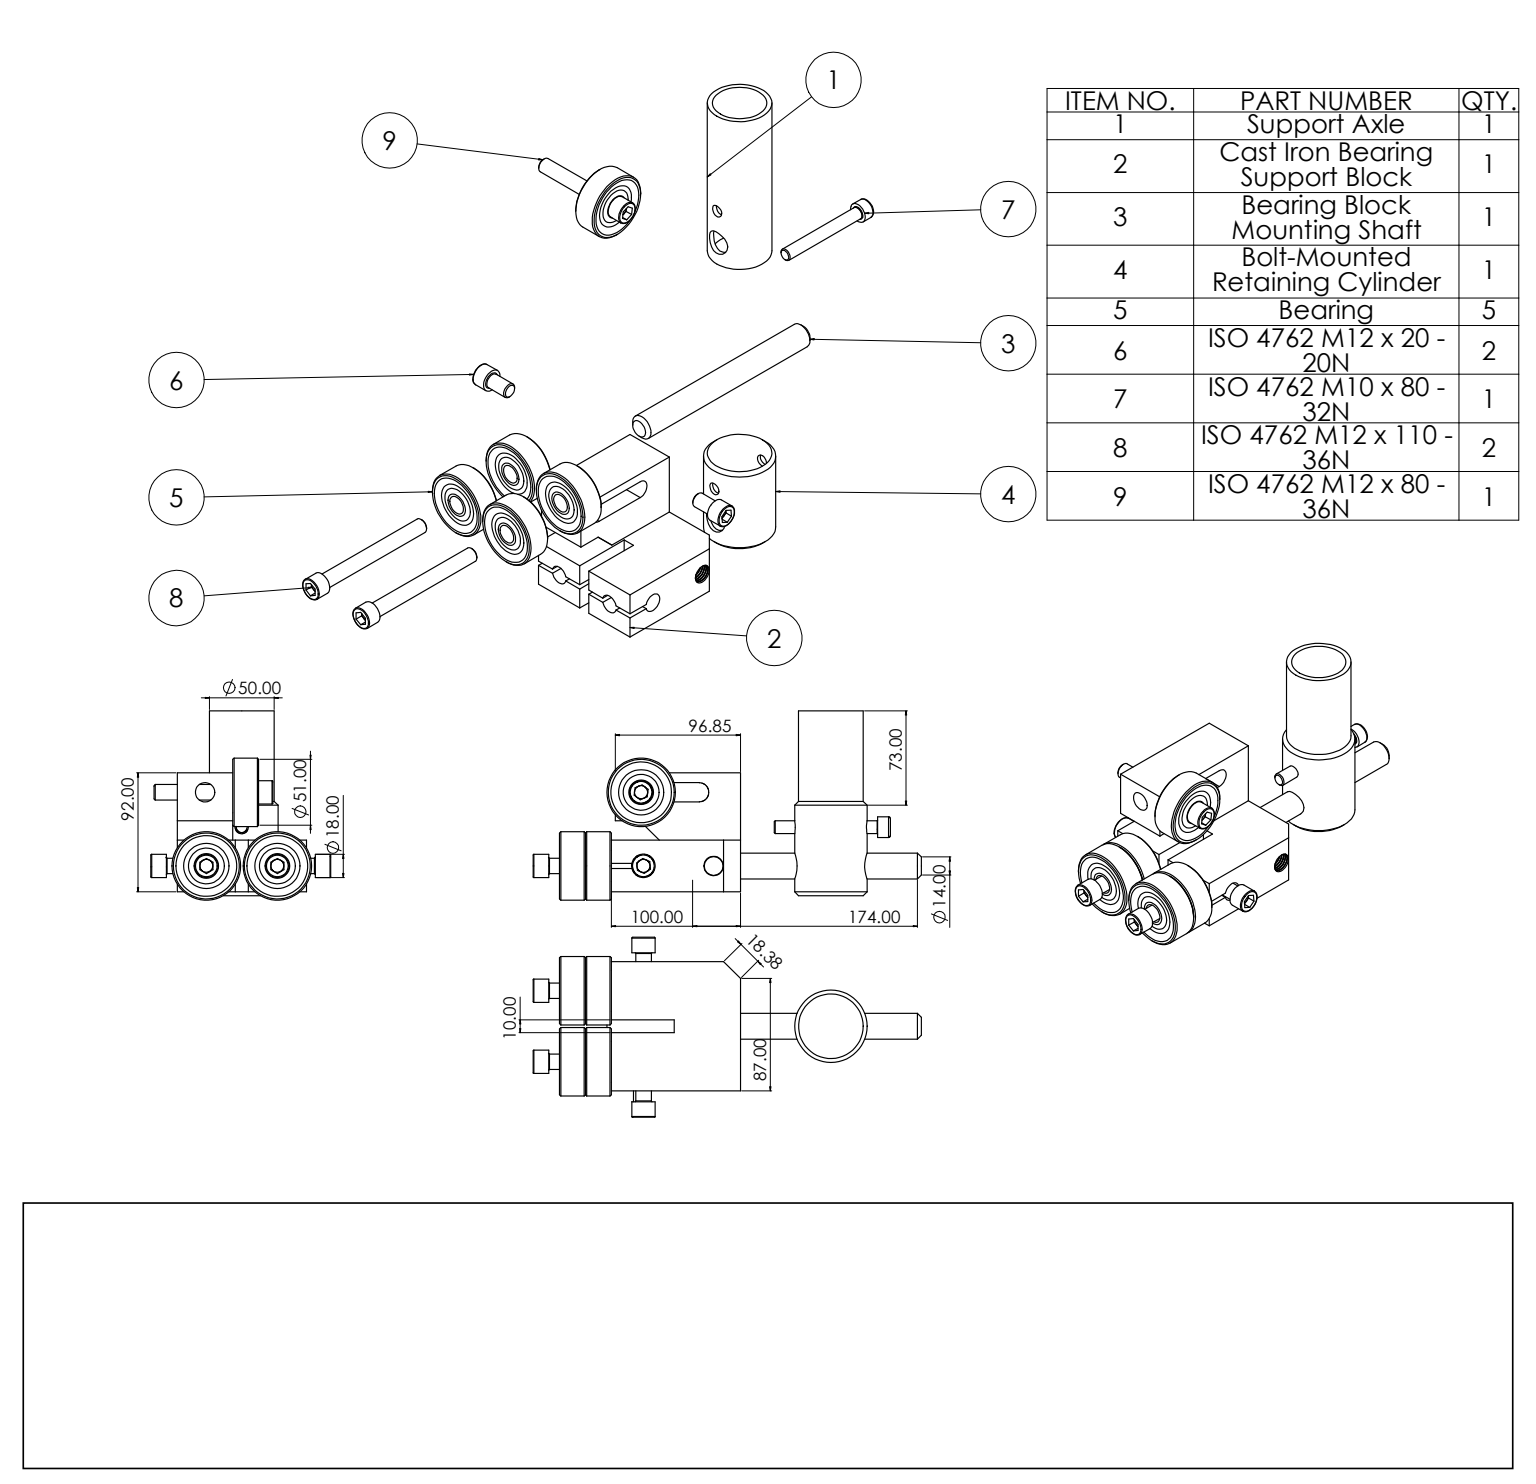
ISO-10303-21;
HEADER;
FILE_DESCRIPTION (('STEP AP214'),
    '1' );
FILE_NAME ('MAS-314',
    '2026-10-19T17:36:30',
    ( '' ),
    ( '' ),
    'SwSTEP 2.0',
    'SolidWorks 2025',
    '' );
FILE_SCHEMA (( 'AUTOMOTIVE_DESIGN' ));
ENDSEC;

DATA;
#1 = CARTESIAN_POINT ( 'NONE',  ( 38.97500000054622404, 24.28113015263587471, 84.90069139318163138 ) ) ;
#2 = CARTESIAN_POINT ( 'NONE',  ( 27.17500000054621978, 26.19570976099943493, 86.29171490190961435 ) ) ;
#3 = CARTESIAN_POINT ( 'NONE',  ( 23.09999999999998721, 22.43689772174679575, 83.29316153445363113 ) ) ;
#4 = CARTESIAN_POINT ( 'NONE',  ( 19.93750000027310421, 20.00000000000000355, 98.18490835945361539 ) ) ;
#5 = CARTESIAN_POINT ( 'NONE',  ( 32.97500000054622404, 24.28113015263587471, 84.90069139318163138 ) ) ;
#6 = ORIENTED_EDGE ( 'NONE', *, *, #525, .T. ) ;
#7 = CIRCLE ( 'NONE', #4871, 25.00000000000000000 ) ;
#8 = PRODUCT ( 'socket head cap screw_iso_ISO 4762 M12 x 20 - 20N', 'socket head cap screw_iso_ISO 4762 M12 x 20 - 20N', '', ( #2148 ) ) ;
#9 = DIRECTION ( 'NONE',  ( -0.000000000000000000, -0.000000000000000000, -1.000000000000000000 ) ) ;
#10 = VERTEX_POINT ( 'NONE', #4037 ) ;
#11 = CARTESIAN_POINT ( 'NONE',  ( 49.45000000109246940, 24.40838939219354842, 96.86078899226572503 ) ) ;
#12 = ORIENTED_EDGE ( 'NONE', *, *, #10107, .F. ) ;
#13 = CARTESIAN_POINT ( 'NONE',  ( 43.29999999999999005, 26.37988106264029398, 86.15790661882942914 ) ) ;
#14 = DIRECTION ( 'NONE',  ( -0.000000000000000000, -0.000000000000000000, -1.000000000000000000 ) ) ;
#15 = AXIS2_PLACEMENT_3D ( 'NONE', #3653, #6573, #1689 ) ;
#16 = CARTESIAN_POINT ( 'NONE',  ( 43.67500000054621978, 24.28113015263587116, 96.68563167572563088 ) ) ;
#17 = FACE_OUTER_BOUND ( 'NONE', #5721, .T. ) ;
#18 = EDGE_CURVE ( 'NONE', #5684, #6252, #9693, .T. ) ;
#19 = CARTESIAN_POINT ( 'NONE',  ( -50.00000000000001421, 18.00000000000000355, 188.4007504869563263 ) ) ;
#20 = CARTESIAN_POINT ( 'NONE',  ( 46.77500000054622831, 17.63344945572770328, 83.50966788445364841 ) ) ;
#21 = CARTESIAN_POINT ( 'NONE',  ( 48.49999999999999289, 12.11403331821300533, 90.79316153445363113 ) ) ;
#22 = DIRECTION ( 'NONE',  ( -1.000000000000000000, -9.251858538542971828E-16, 0.000000000000000000 ) ) ;
#23 = CARTESIAN_POINT ( 'NONE',  ( 44.29999999999999005, 13.62011893735970958, 95.42841645007781892 ) ) ;
#24 = ORIENTED_EDGE ( 'NONE', *, *, #11626, .T. ) ;
#25 = CARTESIAN_POINT ( 'NONE',  ( 31.75000000109246656, 17.56310227825320425, 98.29316153445363113 ) ) ;
#26 = CARTESIAN_POINT ( 'NONE',  ( 5.000000000000000888, 49.66980702654861801, -24.49489742783178059 ) ) ;
#27 = ORIENTED_EDGE ( 'NONE', *, *, #5795, .F. ) ;
#28 = EDGE_CURVE ( 'NONE', #7100, #9959, #2772, .T. ) ;
#29 = CIRCLE ( 'NONE', #3272, 28.00000000000000000 ) ;
#30 = ORIENTED_EDGE ( 'NONE', *, *, #9025, .T. ) ;
#31 = CARTESIAN_POINT ( 'NONE',  ( -27.49999999999999645, 20.00000000000000355, 169.9999999999999716 ) ) ;
#32 = CARTESIAN_POINT ( 'NONE',  ( -2.507735966467860678, 54.33796433351858468, -24.87540749666489148 ) ) ;
#33 = CARTESIAN_POINT ( 'NONE',  ( -2.000000000000015543, 20.00000000000000355, 83.29316153445364534 ) ) ;
#34 = CARTESIAN_POINT ( 'NONE',  ( 36.27500000054623541, 12.34168156654572535, 90.79316153445363113 ) ) ;
#35 = CARTESIAN_POINT ( 'NONE',  ( 34.77500000054622831, 17.63344945572770328, 83.50966788445364841 ) ) ;
#36 = B_SPLINE_CURVE_WITH_KNOTS ( 'NONE', 3,
 ( #5460, #12302, #630, #1640, #3542, #1581, #10446, #9451, #12364, #9328, #4495, #7414, #1699, #2590, #753, #3601, #7540, #9388 ),
 .UNSPECIFIED., .F., .F.,
 ( 4, 2, 2, 2, 2, 2, 2, 2, 4 ),
 ( 0.000000000000000000, 0.0009797303413002214287, 0.001959460682600442857, 0.002939191023900664286, 0.003918921365200885715, 0.004898651706501107143, 0.005878382047801328572, 0.006858112389101550001, 0.007837842730401771429 ),
 .UNSPECIFIED. ) ;
#37 = CARTESIAN_POINT ( 'NONE',  ( 35.55000000109245661, 22.43689772174678154, 98.29316153445364534 ) ) ;
#38 = CARTESIAN_POINT ( 'NONE',  ( 9.468091998436410250, 23.23472460790263838, -26.35081933702187129 ) ) ;
#39 = DIRECTION ( 'NONE',  ( 0.000000000000000000, -1.000000000000000000, 1.039664082171044875E-15 ) ) ;
#40 = ORIENTED_EDGE ( 'NONE', *, *, #1850, .F. ) ;
#41 = CARTESIAN_POINT ( 'NONE',  ( 48.57500000054622546, 13.80429023900056684, 86.29171490190961435 ) ) ;
#42 = CARTESIAN_POINT ( 'NONE',  ( -5.000000000000000000, 50.00000000000000000, 24.49489742783178414 ) ) ;
#43 = ORIENTED_EDGE ( 'NONE', *, *, #4823, .T. ) ;
#44 = DIRECTION ( 'NONE',  ( 0.000000000000000000, 0.000000000000000000, -1.000000000000000000 ) ) ;
#45 = DIRECTION ( 'NONE',  ( -1.000000000000000000, 0.000000000000000000, -0.000000000000000000 ) ) ;
#46 = ORIENTED_EDGE ( 'NONE', *, *, #5665, .T. ) ;
#47 = ORIENTED_EDGE ( 'NONE', *, *, #4033, .T. ) ;
#48 = CARTESIAN_POINT ( 'NONE',  ( 43.05000000109246372, 27.13292387221364876, 88.47553407664153724 ) ) ;
#49 = EDGE_CURVE ( 'NONE', #9941, #4353, #11739, .T. ) ;
#50 = DIRECTION ( 'NONE',  ( -0.000000000000000000, -0.000000000000000000, 1.000000000000000000 ) ) ;
#51 = CARTESIAN_POINT ( 'NONE',  ( 6.614339767079327359, 27.50003396314175674, 91.05027562884485803 ) ) ;
#52 = CARTESIAN_POINT ( 'NONE',  ( 37.79999999999998295, 24.40838939219354842, 96.86078899226572503 ) ) ;
#53 = VECTOR ( 'NONE', #12398, 999.9999999999998863 ) ;
#54 = CARTESIAN_POINT ( 'NONE',  ( 49.99999999999998579, 22.00000000000000000, 169.9999999999999716 ) ) ;
#55 = CARTESIAN_POINT ( 'NONE',  ( 1.302272420532246455, 45.16122859629937381, -20.96210264449279137 ) ) ;
#56 = CARTESIAN_POINT ( 'NONE',  ( 90.00000000000000000, 0.000000000000000000, 4.171999999999999709 ) ) ;
#57 = FACE_OUTER_BOUND ( 'NONE', #633, .T. ) ;
#58 = VERTEX_POINT ( 'NONE', #304 ) ;
#59 = CARTESIAN_POINT ( 'NONE',  ( 37.25000000109246656, 27.13292387221364876, 93.11078899226573924 ) ) ;
#60 = EDGE_CURVE ( 'NONE', #174, #10109, #7975, .T. ) ;
#61 = CARTESIAN_POINT ( 'NONE',  ( 23.07500000054622546, 24.28113015263587471, 84.90069139318163138 ) ) ;
#62 = CARTESIAN_POINT ( 'NONE',  ( 23.85000000109246443, 15.59161060780645691, 96.86078899226572503 ) ) ;
#63 = VECTOR ( 'NONE', #11751, 1000.000000000000000 ) ;
#64 = CARTESIAN_POINT ( 'NONE',  ( 37.57500000054622546, 24.28113015263587116, 96.68563167572563088 ) ) ;
#65 = CARTESIAN_POINT ( 'NONE',  ( 21.57500000054622546, 26.19570976099943493, 95.29460816699764791 ) ) ;
#66 = CARTESIAN_POINT ( 'NONE',  ( 21.49999999999998224, 27.88596668178699645, 90.79316153445363113 ) ) ;
#67 = EDGE_CURVE ( 'NONE', #6224, #4669, #12253, .T. ) ;
#68 = CARTESIAN_POINT ( 'NONE',  ( 31.47500000054623115, 26.19570976099943493, 95.29460816699764791 ) ) ;
#69 = ORIENTED_EDGE ( 'NONE', *, *, #4429, .F. ) ;
#70 = LINE ( 'NONE', #9907, #9738 ) ;
#71 = ORIENTED_EDGE ( 'NONE', *, *, #4541, .F. ) ;
#72 = DIRECTION ( 'NONE',  ( 0.000000000000000000, 0.000000000000000000, 1.000000000000000000 ) ) ;
#73 = EDGE_LOOP ( 'NONE', ( #2091, #4719, #3113, #69, #4677 ) ) ;
#74 = CIRCLE ( 'NONE', #4934, 1.499999999999999556 ) ;
#75 = EDGE_CURVE ( 'NONE', #1856, #7546, #10580, .T. ) ;
#76 =( NAMED_UNIT ( * ) SI_UNIT ( $, .STERADIAN. ) SOLID_ANGLE_UNIT ( ) );
#77 = DIRECTION ( 'NONE',  ( 1.000000000000000000, -0.000000000000000000, -0.000000000000000000 ) ) ;
#78 = AXIS2_PLACEMENT_3D ( 'NONE', #6166, #576, #8319 ) ;
#79 = CARTESIAN_POINT ( 'NONE',  ( -2.000000000000015543, 20.00000000000000355, 90.79316153445363113 ) ) ;
#80 = CARTESIAN_POINT ( 'NONE',  ( 44.17500000054621978, 13.80429023900056507, 95.29460816699764791 ) ) ;
#81 = CARTESIAN_POINT ( 'NONE',  ( 39.95000000109245519, 13.62011893735970958, 95.42841645007781892 ) ) ;
#82 = DIRECTION ( 'NONE',  ( 0.000000000000000000, 0.000000000000000000, -1.000000000000000000 ) ) ;
#83 = CARTESIAN_POINT ( 'NONE',  ( 45.47500000054622404, 26.92701409722686634, 93.04388485072563242 ) ) ;
#84 = CARTESIAN_POINT ( 'NONE',  ( 45.29999999999999005, 26.37988106264029398, 86.15790661882942914 ) ) ;
#86 = ADVANCED_FACE ( 'NONE', ( #9056 ), #3026, .F. ) ;
#85 = AXIS2_PLACEMENT_3D ( 'NONE', #8229, #8169, #12160 ) ;
#87 = CARTESIAN_POINT ( 'NONE',  ( 44.99999999999999289, 20.00000000000000355, 83.29316153445364534 ) ) ;
#88 = CARTESIAN_POINT ( 'NONE',  ( 44.09999999999999432, 17.56310227825318648, 98.29316153445363113 ) ) ;
#89 = ORIENTED_EDGE ( 'NONE', *, *, #5986, .F. ) ;
#90 = CIRCLE ( 'NONE', #7986, 25.00000000000000000 ) ;
#91 = CARTESIAN_POINT ( 'NONE',  ( 31.65000000109246514, 20.00000000000000355, 98.29316153445363113 ) ) ;
#92 = DIRECTION ( 'NONE',  ( -1.000000000000000000, 0.000000000000000000, 0.000000000000000000 ) ) ;
#93 = EDGE_LOOP ( 'NONE', ( #11616, #6758, #10652, #3781, #4940 ) ) ;
#94 = EDGE_CURVE ( 'NONE', #11777, #315, #4411, .T. ) ;
#95 = ORIENTED_EDGE ( 'NONE', *, *, #9864, .T. ) ;
#96 = DIRECTION ( 'NONE',  ( 1.000000000000000000, -0.000000000000000000, -0.000000000000000000 ) ) ;
#97 = CARTESIAN_POINT ( 'NONE',  ( -4.999999999999999112, 50.32713193883511593, -24.49489742783179125 ) ) ;
#98 = VECTOR ( 'NONE', #4798, 1000.000000000000000 ) ;
#99 = CARTESIAN_POINT ( 'NONE',  ( 0.000000000000000000, 0.000000000000000000, -28.00000000000000355 ) ) ;
#100 = EDGE_CURVE ( 'NONE', #1932, #332, #3178, .T. ) ;
#101 = CARTESIAN_POINT ( 'NONE',  ( 38.37500000054622973, 13.07298590277314432, 88.54243821818161564 ) ) ;
#102 = CARTESIAN_POINT ( 'NONE',  ( 31.17500000054621978, 26.19570976099943493, 86.29171490190961435 ) ) ;
#103 = CARTESIAN_POINT ( 'NONE',  ( 34.65000000109246514, 20.00000000000000355, 83.29316153445364534 ) ) ;
#104 = CARTESIAN_POINT ( 'NONE',  ( -9.477880355945590196, 23.25612560302911902, 18.74165831626246970 ) ) ;
#105 = FACE_OUTER_BOUND ( 'NONE', #3848, .T. ) ;
#106 = ORIENTED_EDGE ( 'NONE', *, *, #5900, .F. ) ;
#107 = CARTESIAN_POINT ( 'NONE',  ( 49.77500000054621410, 22.36655054427230027, 98.07665518445361386 ) ) ;
#108 = CYLINDRICAL_SURFACE ( 'NONE', #8780, 6.000000000000003553 ) ;
#109 = LINE ( 'NONE', #11712, #6790 ) ;
#110 = VERTEX_POINT ( 'NONE', #7455 ) ;
#111 = CARTESIAN_POINT ( 'NONE',  ( 31.89339828220178674, 12.50000000000000888, 140.6066017177982133 ) ) ;
#112 = AXIS2_PLACEMENT_3D ( 'NONE', #4795, #6504, #8414 ) ;
#113 = VERTEX_POINT ( 'NONE', #8411 ) ;
#114 = EDGE_LOOP ( 'NONE', ( #10765, #3378, #1409, #9629, #7659 ) ) ;
#115 = FACE_OUTER_BOUND ( 'NONE', #4658, .T. ) ;
#116 = CARTESIAN_POINT ( 'NONE',  ( -34.72841614740048044, 22.00000000000000000, 152.2284161474004520 ) ) ;
#117 = PRODUCT_DEFINITION_SHAPE ( 'NONE', 'NONE',  #10531 ) ;
#118 = CARTESIAN_POINT ( 'NONE',  ( 6.732665147703623454, 27.39438278699427087, 92.07235497779568334 ) ) ;
#119 = CARTESIAN_POINT ( 'NONE',  ( 1.500000000000001332, 0.000000000000000000, 0.000000000000000000 ) ) ;
#120 = CARTESIAN_POINT ( 'NONE',  ( -3.766911610146119305, 46.69571375074811925, -24.71569286637712892 ) ) ;
#121 = DIRECTION ( 'NONE',  ( 0.000000000000000000, -1.000000000000000000, 1.039664082171044481E-15 ) ) ;
#122 = CARTESIAN_POINT ( 'NONE',  ( 4.337695533240938595, 47.49144378315899928, 27.66258726422904246 ) ) ;
#123 = CARTESIAN_POINT ( 'NONE',  ( 43.27500000054623541, 27.65831843345427998, 90.79316153445363113 ) ) ;
#124 = AXIS2_PLACEMENT_3D ( 'NONE', #8869, #5257, #7026 ) ;
#125 = CARTESIAN_POINT ( 'NONE',  ( 27.49999999999999645, 20.00000000000000355, 169.9999999999999716 ) ) ;
#126 = ORIENTED_EDGE ( 'NONE', *, *, #9586, .F. ) ;
#127 = PLANE ( 'NONE',  #5041 ) ;
#128 = APPLICATION_PROTOCOL_DEFINITION ( 'draft international standard', 'automotive_design', 1998, #8052 ) ;
#129 = CARTESIAN_POINT ( 'NONE',  ( 46.19999999999998863, 15.59161060780645691, 96.86078899226572503 ) ) ;
#130 = DIRECTION ( 'NONE',  ( 1.000000000000000000, 0.000000000000000000, 0.000000000000000000 ) ) ;
#131 = CARTESIAN_POINT ( 'NONE',  ( 30.37500000054622973, 13.07298590277314432, 88.54243821818161564 ) ) ;
#132 = CARTESIAN_POINT ( 'NONE',  ( 22.17500000054622333, 13.80429023900056507, 95.29460816699764791 ) ) ;
#133 = CARTESIAN_POINT ( 'NONE',  ( 24.89999999999999147, 17.56310227825321135, 83.29316153445363113 ) ) ;
#134 = CARTESIAN_POINT ( 'NONE',  ( -10.00000000000000355, 20.00000000000000355, -22.91287847477919826 ) ) ;
#135 = CARTESIAN_POINT ( 'NONE',  ( 33.07500000054623257, 26.19570976099943493, 86.29171490190961435 ) ) ;
#136 = VERTEX_POINT ( 'NONE', #11263 ) ;
#137 = DIRECTION ( 'NONE',  ( 0.000000000000000000, -0.000000000000000000, 1.000000000000000000 ) ) ;
#138 = EDGE_LOOP ( 'NONE', ( #6362, #6499, #12399, #3015, #10689, #7029 ) ) ;
#139 = EDGE_CURVE ( 'NONE', #6118, #11306, #5452, .T. ) ;
#140 = DIRECTION ( 'NONE',  ( 1.000000000000000000, -0.000000000000000000, -0.000000000000000000 ) ) ;
#141 = EDGE_LOOP ( 'NONE', ( #2879, #8210, #6869, #7953, #8806, #9023 ) ) ;
#142 = AXIS2_PLACEMENT_3D ( 'NONE', #1198, #5064, #7978 ) ;
#143 = CARTESIAN_POINT ( 'NONE',  ( -3.767068525368503895, 53.30379312071067233, -24.71564595051174607 ) ) ;
#144 = CARTESIAN_POINT ( 'NONE',  ( 6.107750375176497215, 12.05530454078378000, -27.33128490115649711 ) ) ;
#145 = EDGE_CURVE ( 'NONE', #6002, #9969, #12095, .T. ) ;
#146 = CARTESIAN_POINT ( 'NONE',  ( 38.17500000054622689, 13.80429023900056507, 95.29460816699764791 ) ) ;
#147 = DIRECTION ( 'NONE',  ( 0.000000000000000000, 0.000000000000000000, -1.000000000000000000 ) ) ;
#148 = CARTESIAN_POINT ( 'NONE',  ( 26.79999999999998650, 15.59161060780646046, 84.72553407664153724 ) ) ;
#149 = CARTESIAN_POINT ( 'NONE',  ( 42.07500000054622546, 15.71886984736413417, 96.68563167572563088 ) ) ;
#150 = CARTESIAN_POINT ( 'NONE',  ( 43.89999999999999147, 22.43689772174679575, 98.29316153445363113 ) ) ;
#151 = CIRCLE ( 'NONE', #9264, 7.500000000000000000 ) ;
#152 = LINE ( 'NONE', #11692, #6762 ) ;
#153 = FACE_BOUND ( 'NONE', #206, .T. ) ;
#154 = ORIENTED_EDGE ( 'NONE', *, *, #8754, .F. ) ;
#155 = CARTESIAN_POINT ( 'NONE',  ( 33.65000000109246514, 20.00000000000000355, 98.29316153445363113 ) ) ;
#156 = DIRECTION ( 'NONE',  ( 1.000000000000000000, 0.000000000000000000, 0.000000000000000000 ) ) ;
#157 = EDGE_LOOP ( 'NONE', ( #10201, #8634, #9210, #7261, #8098 ) ) ;
#158 = ORIENTED_EDGE ( 'NONE', *, *, #6876, .T. ) ;
#159 = CARTESIAN_POINT ( 'NONE',  ( 25.65000000109246514, 20.00000000000000355, 98.29316153445363113 ) ) ;
#160 = EDGE_CURVE ( 'NONE', #6466, #7533, #9507, .T. ) ;
#161 = CONICAL_SURFACE ( 'NONE', #12112, 5.057500000000000107, 1.047197551196592302 ) ;
#162 = DIRECTION ( 'NONE',  ( 1.000000000000000000, -0.000000000000000000, -0.000000000000000000 ) ) ;
#163 = CARTESIAN_POINT ( 'NONE',  ( 48.09999999999999432, 17.56310227825322556, 98.29316153445364534 ) ) ;
#164 = CARTESIAN_POINT ( 'NONE',  ( 32.87500000054622973, 22.36655054427230382, 83.50966788445364841 ) ) ;
#165 = CARTESIAN_POINT ( 'NONE',  ( 29.87500000054622618, 20.00000000000000355, 98.07665518445361386 ) ) ;
#166 = CARTESIAN_POINT ( 'NONE',  ( -1.612284376581284429, 54.74427448601975499, 27.95519242099699397 ) ) ;
#167 = CARTESIAN_POINT ( 'NONE',  ( 44.05000000109246372, 12.86707612778636012, 93.11078899226572503 ) ) ;
#168 = DIRECTION ( 'NONE',  ( 0.000000000000000000, -0.000000000000000000, -1.000000000000000000 ) ) ;
#169 = VERTEX_POINT ( 'NONE', #4475 ) ;
#170 = CARTESIAN_POINT ( 'NONE',  ( -31.74999999999995737, 0.000000000000000000, 0.000000000000000000 ) ) ;
#171 = CARTESIAN_POINT ( 'NONE',  ( 21.99999999999998934, 20.00000000000000355, 98.29316153445363113 ) ) ;
#172 = ORIENTED_EDGE ( 'NONE', *, *, #1724, .F. ) ;
#173 = DIRECTION ( 'NONE',  ( 0.000000000000000000, 0.000000000000000000, 1.000000000000000000 ) ) ;
#174 = VERTEX_POINT ( 'NONE', #10304 ) ;
#175 = EDGE_CURVE ( 'NONE', #10286, #4797, #4025, .T. ) ;
#176 = ORIENTED_EDGE ( 'NONE', *, *, #7484, .F. ) ;
#177 = VECTOR ( 'NONE', #2626, 1000.000000000000000 ) ;
#178 = LINE ( 'NONE', #1320, #6017 ) ;
#179 = EDGE_CURVE ( 'NONE', #6763, #7138, #1054, .T. ) ;
#180 = CARTESIAN_POINT ( 'NONE',  ( 9.920725400334921673, 21.28151498972171751, 98.18721253656565295 ) ) ;
#181 = LINE ( 'NONE', #4040, #1401 ) ;
#182 = DIRECTION ( 'NONE',  ( -0.7071067811865524577, 0.000000000000000000, -0.7071067811865426878 ) ) ;
#183 = CARTESIAN_POINT ( 'NONE',  ( 4.999999999999999112, 49.83503777815744940, -20.39607805437113441 ) ) ;
#184 = FACE_OUTER_BOUND ( 'NONE', #10225, .T. ) ;
#185 = CONICAL_SURFACE ( 'NONE', #8085, 25.50000000000000711, 0.7853981633974552734 ) ;
#186 = CARTESIAN_POINT ( 'NONE',  ( 40.67500000054623399, 17.63344945572770328, 83.50966788445364841 ) ) ;
#187 = DIRECTION ( 'NONE',  ( 0.000000000000000000, 0.000000000000000000, 1.000000000000000000 ) ) ;
#188 = VERTEX_POINT ( 'NONE', #5686 ) ;
#189 = EDGE_CURVE ( 'NONE', #5728, #3198, #1007, .T. ) ;
#190 =( GEOMETRIC_REPRESENTATION_CONTEXT ( 3 ) GLOBAL_UNCERTAINTY_ASSIGNED_CONTEXT ( ( #2001 ) ) GLOBAL_UNIT_ASSIGNED_CONTEXT ( ( #12461, #11571, #6744 ) ) REPRESENTATION_CONTEXT ( 'NONE', 'WORKASPACE' ) );
#191 = DIRECTION ( 'NONE',  ( -1.000000000000000000, 0.000000000000000000, -0.000000000000000000 ) ) ;
#192 = AXIS2_PLACEMENT_3D ( 'NONE', #3678, #11483, #9714 ) ;
#193 = CARTESIAN_POINT ( 'NONE',  ( 20.47500000054622404, 13.07298590277314432, 88.54243821818161564 ) ) ;
#194 = CYLINDRICAL_SURFACE ( 'NONE', #2295, 10.00000000000000355 ) ;
#195 = CARTESIAN_POINT ( 'NONE',  ( 32.57500000054623257, 15.71886984736413773, 84.90069139318163138 ) ) ;
#196 = CIRCLE ( 'NONE', #3434, 25.00000000000000000 ) ;
#197 = CARTESIAN_POINT ( 'NONE',  ( 4.153883524164314167, 10.89765663934413276, -24.65439000785841372 ) ) ;
#198 = CARTESIAN_POINT ( 'NONE',  ( 23.79999999999998650, 24.40838939219354842, 96.86078899226572503 ) ) ;
#199 = CARTESIAN_POINT ( 'NONE',  ( 4.999999999999997335, 20.00000000000000000, 145.0000000000000000 ) ) ;
#200 = CARTESIAN_POINT ( 'NONE',  ( 32.27500000054622831, 12.34168156654572535, 90.79316153445363113 ) ) ;
#201 = ORIENTED_EDGE ( 'NONE', *, *, #4123, .F. ) ;
#202 = DIRECTION ( 'NONE',  ( -1.000000000000000000, -0.000000000000000000, -0.000000000000000000 ) ) ;
#203 = FACE_OUTER_BOUND ( 'NONE', #1468, .T. ) ;
#204 = ORIENTED_EDGE ( 'NONE', *, *, #7341, .T. ) ;
#205 = CARTESIAN_POINT ( 'NONE',  ( 4.736559457325700606, 51.60997564292328121, 27.59650980994295466 ) ) ;
#206 = EDGE_LOOP ( 'NONE', ( #5971, #3892 ) ) ;
#207 = DIRECTION ( 'NONE',  ( 1.000000000000000000, 0.000000000000000000, 0.000000000000000000 ) ) ;
#208 = CARTESIAN_POINT ( 'NONE',  ( 5.000000000000000000, -4.685197434473812983, 6.938893903907228378E-15 ) ) ;
#209 = DIRECTION ( 'NONE',  ( -0.000000000000000000, -0.000000000000000000, -1.000000000000000000 ) ) ;
#210 = CARTESIAN_POINT ( 'NONE',  ( 39.07500000054622546, 24.28113015263587471, 84.90069139318163138 ) ) ;
#211 = CARTESIAN_POINT ( 'NONE',  ( 40.35000000109246088, 13.62011893735970958, 86.15790661882942914 ) ) ;
#212 = ADVANCED_FACE ( 'NONE', ( #2945 ), #5804, .F. ) ;
#213 = CARTESIAN_POINT ( 'NONE',  ( -4.680751350184292114, 48.23435024407273630, -27.60606166384445714 ) ) ;
#214 = CARTESIAN_POINT ( 'NONE',  ( 42.17500000054623399, 13.80429023900056507, 95.29460816699764791 ) ) ;
#215 = CARTESIAN_POINT ( 'NONE',  ( 43.79999999999999005, 24.40838939219354842, 96.86078899226572503 ) ) ;
#216 = MECHANICAL_DESIGN_GEOMETRIC_PRESENTATION_REPRESENTATION (  '', ( #1626 ), #7294 ) ;
#217 = CARTESIAN_POINT ( 'NONE',  ( 39.59999999999998721, 27.13292387221364876, 93.11078899226573924 ) ) ;
#218 = CARTESIAN_POINT ( 'NONE',  ( -20.00000000000000355, 15.60660171779822569, 137.5000000000000000 ) ) ;
#219 = EDGE_LOOP ( 'NONE', ( #7891, #2813, #3366 ) ) ;
#220 = CARTESIAN_POINT ( 'NONE',  ( 30.85000000109246443, 24.40838939219355197, 84.72553407664153724 ) ) ;
#221 = DIRECTION ( 'NONE',  ( 0.000000000000000000, 0.000000000000000000, -1.000000000000000000 ) ) ;
#222 = ORIENTED_EDGE ( 'NONE', *, *, #49, .T. ) ;
#223 = VERTEX_POINT ( 'NONE', #1985 ) ;
#224 = TOROIDAL_SURFACE ( 'NONE', #9540, 6.599999999999999645, 0.5999999999999999778 ) ;
#225 = CYLINDRICAL_SURFACE ( 'NONE', #7691, 7.499999999999992895 ) ;
#226 = PRODUCT_DEFINITION_SHAPE ( 'NONE', 'NONE',  #5124 ) ;
#227 = CARTESIAN_POINT ( 'NONE',  ( -34.72841614740048044, 22.00000000000000000, 169.9999999999999716 ) ) ;
#228 = PLANE ( 'NONE',  #9406 ) ;
#229 = CARTESIAN_POINT ( 'NONE',  ( 27.97500000054623115, 15.71886984736413417, 96.68563167572563088 ) ) ;
#230 = CARTESIAN_POINT ( 'NONE',  ( 33.87500000054622262, 20.00000000000000355, 98.07665518445361386 ) ) ;
#231 = CARTESIAN_POINT ( 'NONE',  ( -10.00000000000000178, 20.33047844303349905, 18.46618531261938756 ) ) ;
#232 = CARTESIAN_POINT ( 'NONE',  ( 31.89339828220179385, 27.49999999999999645, 140.6066017177982133 ) ) ;
#233 = ORIENTED_EDGE ( 'NONE', *, *, #8654, .T. ) ;
#234 = AXIS2_PLACEMENT_3D ( 'NONE', #11522, #6698, #10625 ) ;
#235 = EDGE_CURVE ( 'NONE', #3714, #6224, #3532, .T. ) ;
#236 = CARTESIAN_POINT ( 'NONE',  ( 49.65000000109246514, 20.00000000000000355, 98.29316153445363113 ) ) ;
#237 = LINE ( 'NONE', #8918, #9432 ) ;
#238 = ORIENTED_EDGE ( 'NONE', *, *, #11054, .T. ) ;
#239 = ORIENTED_EDGE ( 'NONE', *, *, #75, .F. ) ;
#240 = PRODUCT_DEFINITION ( 'UNKNOWN', '', #9002, #6124 ) ;
#241 = CARTESIAN_POINT ( 'NONE',  ( -27.49999999999999645, 12.50000000000001066, 145.0000000000000000 ) ) ;
#242 = CARTESIAN_POINT ( 'NONE',  ( -1.002883791299520887E-19, 10.00000000000000000, -25.00000000000000000 ) ) ;
#243 = EDGE_CURVE ( 'NONE', #9959, #918, #9739, .T. ) ;
#244 = DIRECTION ( 'NONE',  ( 0.000000000000000000, 0.000000000000000000, 1.000000000000000000 ) ) ;
#245 = LINE ( 'NONE', #7790, #3780 ) ;
#246 = CARTESIAN_POINT ( 'NONE',  ( 9.617918704988914769, 22.74817246778840385, 83.81039675207235007 ) ) ;
#247 = CARTESIAN_POINT ( 'NONE',  ( 5.000000000000000000, 50.00000000000000000, -24.49489742783178414 ) ) ;
#248 = CARTESIAN_POINT ( 'NONE',  ( 31.03600000000003689, 0.000000000000000000, 6.000000000000003553 ) ) ;
#249 = DIRECTION ( 'NONE',  ( 1.000000000000000000, -0.000000000000000000, -0.000000000000000000 ) ) ;
#250 = CARTESIAN_POINT ( 'NONE',  ( -2.507472281498270394, 45.66193322363204032, 27.88882835875018174 ) ) ;
#251 = CARTESIAN_POINT ( 'NONE',  ( 44.67500000054623399, 17.63344945572770328, 83.50966788445364841 ) ) ;
#252 = CARTESIAN_POINT ( 'NONE',  ( 3.053062343563090142, 46.02672757820099037, 20.77871069257179215 ) ) ;
#253 = ORIENTED_EDGE ( 'NONE', *, *, #2837, .F. ) ;
#254 = LINE ( 'NONE', #4112, #5840 ) ;
#255 = ADVANCED_FACE ( 'NONE', ( #3893 ), #3702, .T. ) ;
#256 = CONTEXT_DEPENDENT_SHAPE_REPRESENTATION ( #10162, #1033 ) ;
#257 = CARTESIAN_POINT ( 'NONE',  ( 21.87500000054622618, 20.00000000000000355, 98.07665518445361386 ) ) ;
#258 = CARTESIAN_POINT ( 'NONE',  ( 121.0360000000000156, 0.000000000000000000, 0.000000000000000000 ) ) ;
#259 = CARTESIAN_POINT ( 'NONE',  ( 31.27500000054622831, 27.65831843345427998, 90.79316153445363113 ) ) ;
#261 = EDGE_CURVE ( 'NONE', #12355, #6453, #10609, .T. ) ;
#260 =( BOUNDED_CURVE ( )  B_SPLINE_CURVE ( 2, ( #4396, #8213, #3321, #10235, #5421, #7127, #353, #8339, #12082, #5358, #12143 ),
 .UNSPECIFIED., .F., .F. ) 
 B_SPLINE_CURVE_WITH_KNOTS ( ( 3, 2, 2, 2, 2, 3 ),
 ( 0.4333333333333334592, 0.4400000000000000577, 0.4466666666666667118, 0.4533333333333333104, 0.4600000000000000200, 0.4666666666666666186 ),
 .UNSPECIFIED. ) 
 CURVE ( )  GEOMETRIC_REPRESENTATION_ITEM ( )  RATIONAL_B_SPLINE_CURVE ( ( 0.9999999999999992228, 0.9510565162951543083, 1.000000000000000000, 0.9510565162951535312, 1.000000000000000000, 0.9510565162951535312, 1.000000000000000000, 0.9510565162951535312, 1.000000000000000000, 0.9510565162951539753, 0.9999999999999995559 ) ) 
 REPRESENTATION_ITEM ( '' )  );
#262 = CARTESIAN_POINT ( 'NONE',  ( 22.97500000054622049, 22.36655054427230382, 83.50966788445364841 ) ) ;
#263 = CARTESIAN_POINT ( 'NONE',  ( 23.19999999999998863, 24.40838939219355197, 84.72553407664153724 ) ) ;
#264 = LINE ( 'NONE', #9078, #7887 ) ;
#265 = CARTESIAN_POINT ( 'NONE',  ( 24.47500000054623115, 13.80429023900056684, 86.29171490190961435 ) ) ;
#266 = EDGE_LOOP ( 'NONE', ( #3910, #10160, #3333, #10971 ) ) ;
#267 = CARTESIAN_POINT ( 'NONE',  ( 6.000000000000000000, -2.919948986426538884, -5.057499999999997442 ) ) ;
#268 = ORIENTED_EDGE ( 'NONE', *, *, #60, .F. ) ;
#269 = CARTESIAN_POINT ( 'NONE',  ( 3.052391101563580733, 53.97379179909159319, 27.83448159811773692 ) ) ;
#270 = ORIENTED_EDGE ( 'NONE', *, *, #9752, .F. ) ;
#271 = DIRECTION ( 'NONE',  ( 0.000000000000000000, 1.000000000000000000, 0.000000000000000000 ) ) ;
#272 = VECTOR ( 'NONE', #1470, 1000.000000000000000 ) ;
#273 = CARTESIAN_POINT ( 'NONE',  ( 40.87500000054622262, 20.00000000000000355, 83.50966788445364841 ) ) ;
#274 = DIRECTION ( 'NONE',  ( 0.000000000000000000, 0.000000000000000000, -1.000000000000000000 ) ) ;
#275 = CARTESIAN_POINT ( 'NONE',  ( -4.491894572514616435, 47.77948379856257333, -27.63764060679477552 ) ) ;
#276 = CARTESIAN_POINT ( 'NONE',  ( 41.69999999999998863, 26.37988106264029398, 95.42841645007781892 ) ) ;
#277 = CARTESIAN_POINT ( 'NONE',  ( 45.77500000054622831, 20.00000000000000355, 98.07665518445361386 ) ) ;
#278 = ORIENTED_EDGE ( 'NONE', *, *, #319, .T. ) ;
#279 = CIRCLE ( 'NONE', #7565, 6.599999999999999645 ) ;
#280 = CARTESIAN_POINT ( 'NONE',  ( 28.65000000109246514, 20.00000000000000355, 83.29316153445364534 ) ) ;
#281 = CARTESIAN_POINT ( 'NONE',  ( 3.052678183968668524, 46.02654057254596154, -24.81443426854575307 ) ) ;
#282 = ORIENTED_EDGE ( 'NONE', *, *, #2101, .F. ) ;
#283 = PLANE ( 'NONE',  #2263 ) ;
#284 = ORIENTED_EDGE ( 'NONE', *, *, #6755, .T. ) ;
#285 = CARTESIAN_POINT ( 'NONE',  ( 5.000000000000000000, 2.342598717236912265, 4.057499999999998330 ) ) ;
#286 = DIRECTION ( 'NONE',  ( -1.000000000000000000, -0.000000000000000000, -0.000000000000000000 ) ) ;
#287 = DIRECTION ( 'NONE',  ( 0.000000000000000000, 0.000000000000000000, 1.000000000000000000 ) ) ;
#288 = VECTOR ( 'NONE', #6310, 1000.000000000000000 ) ;
#289 = PRODUCT_DEFINITION_CONTEXT ( 'detailed design', #1328, 'design' ) ;
#290 = CARTESIAN_POINT ( 'NONE',  ( 31.57500000054622902, 24.28113015263587116, 96.68563167572563088 ) ) ;
#291 = CARTESIAN_POINT ( 'NONE',  ( 28.77500000054622831, 17.63344945572770328, 83.50966788445364841 ) ) ;
#292 = VECTOR ( 'NONE', #10124, 1000.000000000000000 ) ;
#293 = CARTESIAN_POINT ( 'NONE',  ( -3.303835886662602306, 53.76734242787640028, 27.80538831778189746 ) ) ;
#294 = CARTESIAN_POINT ( 'NONE',  ( 20.00000000000003908, 20.00000000000000000, 137.5000000000000000 ) ) ;
#295 = DIRECTION ( 'NONE',  ( 1.000000000000000000, 0.000000000000000000, 0.000000000000000000 ) ) ;
#296 = ORIENTED_EDGE ( 'NONE', *, *, #3871, .F. ) ;
#297 = CARTESIAN_POINT ( 'NONE',  ( 48.77500000054623541, 17.63344945572770328, 83.50966788445364841 ) ) ;
#298 = CARTESIAN_POINT ( 'NONE',  ( 10.00000000000000000, 0.000000000000000000, -5.400000000000001243 ) ) ;
#299 = ORIENTED_EDGE ( 'NONE', *, *, #10711, .T. ) ;
#300 = CARTESIAN_POINT ( 'NONE',  ( -50.00000000000001421, 84.49999999999998579, 146.8533255156881978 ) ) ;
#301 = ORIENTED_EDGE ( 'NONE', *, *, #8138, .T. ) ;
#302 = EDGE_CURVE ( 'NONE', #1347, #9626, #5867, .T. ) ;
#303 = CIRCLE ( 'NONE', #9825, 28.00000000000000355 ) ;
#304 = CARTESIAN_POINT ( 'NONE',  ( 30.65000000109246514, 20.00000000000000355, 83.29316153445364534 ) ) ;
#305 = LINE ( 'NONE', #2067, #7223 ) ;
#306 = CARTESIAN_POINT ( 'NONE',  ( 12.00000000000000000, 8.082668874372530033E-16, 6.599999999999998757 ) ) ;
#307 = CARTESIAN_POINT ( 'NONE',  ( 8.247655429682051675, 25.65770512295588901, 95.72222997683927304 ) ) ;
#308 = DIRECTION ( 'NONE',  ( 0.000000000000000000, 0.000000000000000000, -1.000000000000000000 ) ) ;
#309 =( GEOMETRIC_REPRESENTATION_CONTEXT ( 3 ) GLOBAL_UNCERTAINTY_ASSIGNED_CONTEXT ( ( #9884 ) ) GLOBAL_UNIT_ASSIGNED_CONTEXT ( ( #2929, #7943, #11807 ) ) REPRESENTATION_CONTEXT ( 'NONE', 'WORKASPACE' ) );
#310 = CARTESIAN_POINT ( 'NONE',  ( 8.648152576036682859, 25.03146049264868367, 19.13735728885347243 ) ) ;
#311 = PLANE ( 'NONE',  #124 ) ;
#312 = CIRCLE ( 'NONE', #4165, 9.499999999999994671 ) ;
#313 = CARTESIAN_POINT ( 'NONE',  ( 45.37500000054622973, 26.92701409722686634, 93.04388485072563242 ) ) ;
#314 = CARTESIAN_POINT ( 'NONE',  ( 3.974373595566621731, 46.94861671663893077, 20.62131536938402832 ) ) ;
#315 = VERTEX_POINT ( 'NONE', #6684 ) ;
#316 = CARTESIAN_POINT ( 'NONE',  ( -5.302459511815778903, 11.51535060788542353, -27.49471880134667146 ) ) ;
#317 = ITEM_DEFINED_TRANSFORMATION ( 'NONE', 'NONE', #1501,  #9021 ) ;
#318 = AXIS2_PLACEMENT_3D ( 'NONE', #1742, #10431, #8539 ) ;
#319 = EDGE_CURVE ( 'NONE', #2922, #1223, #6665, .T. ) ;
#320 = CARTESIAN_POINT ( 'NONE',  ( 19.87500000054622262, 20.00000000000000355, 98.07665518445361386 ) ) ;
#321 = CARTESIAN_POINT ( 'NONE',  ( 43.57500000054623257, 26.19570976099943493, 95.29460816699764791 ) ) ;
#322 = CARTESIAN_POINT ( 'NONE',  ( 31.17500000054622689, 26.92701409722686634, 88.54243821818162985 ) ) ;
#323 = CARTESIAN_POINT ( 'NONE',  ( 20.07500000054622546, 15.71886984736413417, 96.68563167572563088 ) ) ;
#324 = DIRECTION ( 'NONE',  ( -1.000000000000000000, -0.000000000000000000, -0.000000000000000000 ) ) ;
#325 = AXIS2_PLACEMENT_3D ( 'NONE', #1284, #11686, #5158 ) ;
#326 = CARTESIAN_POINT ( 'NONE',  ( 27.37500000054622973, 26.92701409722686634, 93.04388485072563242 ) ) ;
#327 = ORIENTED_EDGE ( 'NONE', *, *, #6078, .F. ) ;
#328 = PRODUCT_DEFINITION_SHAPE ( 'NONE', 'NONE',  #12555 ) ;
#329 = FACE_OUTER_BOUND ( 'NONE', #219, .T. ) ;
#330 = ORIENTED_EDGE ( 'NONE', *, *, #8043, .T. ) ;
#331 = CARTESIAN_POINT ( 'NONE',  ( 38.69999999999998863, 13.62011893735970958, 86.15790661882942914 ) ) ;
#332 = VERTEX_POINT ( 'NONE', #3766 ) ;
#333 = ADVANCED_FACE ( 'NONE', ( #11509 ), #1613, .T. ) ;
#334 = CARTESIAN_POINT ( 'NONE',  ( 92.00000000000000000, 0.000000000000000000, 0.000000000000000000 ) ) ;
#335 = EDGE_CURVE ( 'NONE', #7072, #5684, #1922, .T. ) ;
#336 =( BOUNDED_CURVE ( )  B_SPLINE_CURVE ( 2, ( #10274, #1591, #10398, #642, #4505, #8380, #11296, #10334, #1651, #701, #4568 ),
 .UNSPECIFIED., .F., .F. ) 
 B_SPLINE_CURVE_WITH_KNOTS ( ( 3, 2, 2, 2, 2, 3 ),
 ( 0.7333333333333332815, 0.7399999999999999911, 0.7466666666666667007, 0.7533333333333331883, 0.7599999999999998979, 0.7666666666666666075 ),
 .UNSPECIFIED. ) 
 CURVE ( )  GEOMETRIC_REPRESENTATION_ITEM ( )  RATIONAL_B_SPLINE_CURVE ( ( 1.000000000000000000, 0.9510565162951535312, 1.000000000000000000, 0.9510565162951535312, 1.000000000000000000, 0.9510565162951535312, 1.000000000000000000, 0.9510565162951535312, 1.000000000000000000, 0.9510565162951543083, 0.9999999999999992228 ) ) 
 REPRESENTATION_ITEM ( '' )  );
#337 = CARTESIAN_POINT ( 'NONE',  ( 39.27500000054622831, 26.92701409722686634, 88.54243821818162985 ) ) ;
#338 = CARTESIAN_POINT ( 'NONE',  ( -0.6576255085612114915, 54.96747678544938509, -27.99413849967543300 ) ) ;
#339 = VECTOR ( 'NONE', #6071, 1000.000000000000000 ) ;
#340 = CARTESIAN_POINT ( 'NONE',  ( -2.643792293865090848, 45.75297423536069630, -27.87524183494957342 ) ) ;
#341 = CARTESIAN_POINT ( 'NONE',  ( 38.17500000054622689, 13.80429023900056507, 95.29460816699764791 ) ) ;
#342 = CARTESIAN_POINT ( 'NONE',  ( 41.09999999999999432, 22.43689772174679575, 83.29316153445363113 ) ) ;
#343 = ADVANCED_FACE ( 'NONE', ( #7768 ), #9322, .F. ) ;
#344 = CARTESIAN_POINT ( 'NONE',  ( 48.27500000054622120, 12.34168156654572535, 90.79316153445363113 ) ) ;
#345 = ORIENTED_EDGE ( 'NONE', *, *, #10306, .T. ) ;
#346 = CARTESIAN_POINT ( 'NONE',  ( 23.15000000109246514, 27.88596668178699645, 90.79316153445363113 ) ) ;
#347 = DIRECTION ( 'NONE',  ( 0.000000000000000000, 1.000000000000000000, -1.336710962791342904E-15 ) ) ;
#348 = TOROIDAL_SURFACE ( 'NONE', #5807, 8.400000000000000355, 0.5999999999999999778 ) ;
#349 = ORIENTED_EDGE ( 'NONE', *, *, #10874, .F. ) ;
#350 = CARTESIAN_POINT ( 'NONE',  ( -9.869694407337590292, 21.64268126127443281, 26.20293780891199020 ) ) ;
#351 = ORIENTED_EDGE ( 'NONE', *, *, #11716, .T. ) ;
#352 = CARTESIAN_POINT ( 'NONE',  ( 1.312675767292145190, 10.06452048457374460, 27.97675868925955811 ) ) ;
#353 = CARTESIAN_POINT ( 'NONE',  ( 36.05000000109246372, 12.86707612778636012, 93.11078899226572503 ) ) ;
#354 = CARTESIAN_POINT ( 'NONE',  ( 48.19999999999998863, 15.59161060780645691, 96.86078899226572503 ) ) ;
#355 = CIRCLE ( 'NONE', #6829, 21.00000000000000000 ) ;
#356 = CARTESIAN_POINT ( 'NONE',  ( 30.47500000054622404, 13.80429023900056684, 86.29171490190961435 ) ) ;
#357 = CARTESIAN_POINT ( 'NONE',  ( 29.27500000054622475, 26.92701409722686634, 88.54243821818162985 ) ) ;
#358 = CARTESIAN_POINT ( 'NONE',  ( 6.000000000000000000, 2.919948986426538884, 5.057499999999996554 ) ) ;
#359 = CARTESIAN_POINT ( 'NONE',  ( 21.85000000109246443, 15.59161060780645691, 96.86078899226572503 ) ) ;
#360 = ORIENTED_EDGE ( 'NONE', *, *, #5907, .F. ) ;
#361 = CARTESIAN_POINT ( 'NONE',  ( 45.95000000109245519, 13.62011893735971135, 95.42841645007781892 ) ) ;
#362 =( LENGTH_UNIT ( ) NAMED_UNIT ( * ) SI_UNIT ( .MILLI., .METRE. ) );
#363 = ORIENTED_EDGE ( 'NONE', *, *, #6657, .F. ) ;
#364 = LINE ( 'NONE', #7846, #8034 ) ;
#365 = ADVANCED_FACE ( 'NONE', ( #7062 ), #4979, .F. ) ;
#366 = ORIENTED_EDGE ( 'NONE', *, *, #12537, .F. ) ;
#367 = VECTOR ( 'NONE', #8369, 1000.000000000000000 ) ;
#368 = CARTESIAN_POINT ( 'NONE',  ( -8.122732253212674891, 14.15824396964088372, -23.64440389997412950 ) ) ;
#369 = CARTESIAN_POINT ( 'NONE',  ( 10.00000000000000533, 19.67046583110989744, -22.91287847477920181 ) ) ;
#370 = FACE_OUTER_BOUND ( 'NONE', #7720, .T. ) ;
#371 = DIRECTION ( 'NONE',  ( 1.000000000000000000, 0.000000000000000000, 0.000000000000000000 ) ) ;
#372 = ADVANCED_FACE ( 'NONE', ( #11955 ), #8150, .F. ) ;
#373 = DIRECTION ( 'NONE',  ( 0.000000000000000000, 0.000000000000000000, -1.000000000000000000 ) ) ;
#374 = CARTESIAN_POINT ( 'NONE',  ( 1.999999999999988010, 20.00000000000000355, 189.9999999999999716 ) ) ;
#375 = CARTESIAN_POINT ( 'NONE',  ( -10.00000000000000355, 20.00000000000000355, 26.15339366124404208 ) ) ;
#376 = CARTESIAN_POINT ( 'NONE',  ( 3.260856397143627294, 29.47603743248158636, -20.75437471433135883 ) ) ;
#377 = CARTESIAN_POINT ( 'NONE',  ( 1.612540704446980389, 45.26432593853714081, 20.93858753690425090 ) ) ;
#378 = VERTEX_POINT ( 'NONE', #285 ) ;
#379 = VECTOR ( 'NONE', #39, 1000.000000000000000 ) ;
#380 = CARTESIAN_POINT ( 'NONE',  ( -2.221358530307614654, 54.49149874209361144, 24.90297606857491175 ) ) ;
#381 = CARTESIAN_POINT ( 'NONE',  ( 6.000000000000000000, -5.258101095580059469E-15, -5.057500000000000995 ) ) ;
#382 = CARTESIAN_POINT ( 'NONE',  ( 44.77500000054622831, 17.63344945572770328, 83.50966788445364841 ) ) ;
#383 = CARTESIAN_POINT ( 'NONE',  ( 33.77500000054622831, 20.00000000000000355, 98.07665518445361386 ) ) ;
#384 = AXIS2_PLACEMENT_3D ( 'NONE', #11930, #5963, #3236 ) ;
#385 = CARTESIAN_POINT ( 'NONE',  ( 8.252517838734652500, 14.33883749563042720, 95.73505295065133680 ) ) ;
#386 = DIRECTION ( 'NONE',  ( 0.000000000000000000, 0.000000000000000000, -1.000000000000000000 ) ) ;
#387 = CYLINDRICAL_SURFACE ( 'NONE', #2812, 7.499999999999992895 ) ;
#388 = CARTESIAN_POINT ( 'NONE',  ( 23.67500000054622333, 22.36655054427230027, 98.07665518445361386 ) ) ;
#389 = ORIENTED_EDGE ( 'NONE', *, *, #1938, .T. ) ;
#390 = AXIS2_PLACEMENT_3D ( 'NONE', #10424, #8591, #2756 ) ;
#391 = EDGE_CURVE ( 'NONE', #3772, #2249, #5044, .T. ) ;
#392 = DIRECTION ( 'NONE',  ( 0.000000000000000000, 0.000000000000000000, -1.000000000000000000 ) ) ;
#393 = ORIENTED_EDGE ( 'NONE', *, *, #1641, .T. ) ;
#394 = EDGE_LOOP ( 'NONE', ( #5603, #4976 ) ) ;
#395 = ORIENTED_EDGE ( 'NONE', *, *, #8626, .F. ) ;
#396 = EDGE_CURVE ( 'NONE', #10590, #5728, #12016, .T. ) ;
#397 = CARTESIAN_POINT ( 'NONE',  ( 39.77500000054621410, 22.36655054427230027, 98.07665518445361386 ) ) ;
#398 = CARTESIAN_POINT ( 'NONE',  ( 2.571758278209441661E-15, 0.000000000000000000, 21.00000000000000000 ) ) ;
#399 = CARTESIAN_POINT ( 'NONE',  ( 6.000000000000000000, -5.839897972853063557, 6.938893903907228378E-15 ) ) ;
#400 = CARTESIAN_POINT ( 'NONE',  ( 37.77500000054622120, 22.36655054427230027, 98.07665518445361386 ) ) ;
#401 = CARTESIAN_POINT ( 'NONE',  ( 34.29999999999996874, 13.62011893735971135, 95.42841645007781892 ) ) ;
#402 = CARTESIAN_POINT ( 'NONE',  ( 47.77500000054622831, 20.00000000000000355, 98.07665518445361386 ) ) ;
#403 = ORIENTED_EDGE ( 'NONE', *, *, #1195, .F. ) ;
#404 = B_SPLINE_CURVE_WITH_KNOTS ( 'NONE', 3,
 ( #9767, #3861, #1078, #7863, #11791, #5958, #7672, #10766, #3097, #11540, #316, #7991, #3349, #6273, #9132, #6089, #8179, #1333, #4302, #3230, #4244, #5262, #2395, #10144, #3291, #10023, #5138, #440 ),
 .UNSPECIFIED., .F., .F.,
 ( 4, 2, 2, 2, 2, 2, 2, 2, 2, 2, 2, 2, 2, 4 ),
 ( 0.03152712852766463569, 0.03251194422550396368, 0.03349675992334329166, 0.03546639131902194764, 0.03645120701686126868, 0.03743602271470059667, 0.03940565411037925264, 0.04039046980821858063, 0.04137528550605790167, 0.04236010120389722966, 0.04334491690173655765, 0.04531454829741522056, 0.04629936399525454854, 0.04728417969309388347 ),
 .UNSPECIFIED. ) ;
#405 = CARTESIAN_POINT ( 'NONE',  ( 25.45000000109246230, 24.40838939219354842, 96.86078899226572503 ) ) ;
#406 = CARTESIAN_POINT ( 'NONE',  ( 0.000000000000000000, 2.919948986426526005, -5.057500000000003659 ) ) ;
#407 = ORIENTED_EDGE ( 'NONE', *, *, #9717, .F. ) ;
#408 = DIRECTION ( 'NONE',  ( -1.000000000000000000, 0.000000000000000000, 0.000000000000000000 ) ) ;
#409 = VERTEX_POINT ( 'NONE', #1238 ) ;
#410 = CARTESIAN_POINT ( 'NONE',  ( 25.05000000109246727, 27.13292387221364876, 88.47553407664153724 ) ) ;
#411 = ADVANCED_FACE ( 'NONE', ( #5172 ), #225, .F. ) ;
#412 = CARTESIAN_POINT ( 'NONE',  ( 41.45000000109246940, 24.40838939219354842, 96.86078899226572503 ) ) ;
#413 = AXIS2_PLACEMENT_3D ( 'NONE', #7308, #9161, #9285 ) ;
#414 = DIRECTION ( 'NONE',  ( -0.000000000000000000, -1.000000000000000000, -0.000000000000000000 ) ) ;
#415 = CARTESIAN_POINT ( 'NONE',  ( 33.27500000054621410, 27.65831843345427998, 90.79316153445363113 ) ) ;
#416 = CARTESIAN_POINT ( 'NONE',  ( 24.07500000054622546, 15.71886984736413417, 96.68563167572563088 ) ) ;
#417 = CARTESIAN_POINT ( 'NONE',  ( 9.355344799098423536, 23.54748521564438235, 26.39119804395479818 ) ) ;
#418 = EDGE_CURVE ( 'NONE', #8662, #3301, #11169, .T. ) ;
#419 = CARTESIAN_POINT ( 'NONE',  ( -2.000000000000015543, 20.00000000000000355, 98.29316153445363113 ) ) ;
#420 = EDGE_LOOP ( 'NONE', ( #3998, #9368 ) ) ;
#421 = CARTESIAN_POINT ( 'NONE',  ( 44.95000000109246940, 26.37988106264029398, 86.15790661882942914 ) ) ;
#422 = DIRECTION ( 'NONE',  ( -0.5000000000000046629, 1.060575238724903587E-16, -0.8660254037844359321 ) ) ;
#423 = ORIENTED_EDGE ( 'NONE', *, *, #10684, .T. ) ;
#424 = CYLINDRICAL_SURFACE ( 'NONE', #1548, 7.499999999999992895 ) ;
#425 = AXIS2_PLACEMENT_3D ( 'NONE', #10021, #6087, #1331 ) ;
#426 = ORIENTED_EDGE ( 'NONE', *, *, #9632, .F. ) ;
#427 = CARTESIAN_POINT ( 'NONE',  ( -6.613021203892899713, 12.47133511838782383, -19.93742635182809053 ) ) ;
#428 = CARTESIAN_POINT ( 'NONE',  ( -0.3295322344531997905, 30.00000000000001066, 25.00000000000001066 ) ) ;
#429 = CARTESIAN_POINT ( 'NONE',  ( 6.000000000000000000, -2.919948986426523341, 5.057500000000002771 ) ) ;
#430 = VECTOR ( 'NONE', #1813, 999.9999999999998863 ) ;
#431 =( LENGTH_UNIT ( ) NAMED_UNIT ( * ) SI_UNIT ( .MILLI., .METRE. ) );
#432 = CARTESIAN_POINT ( 'NONE',  ( -50.00000000000001421, 77.00000000000000000, 101.8533255156881978 ) ) ;
#433 = DIRECTION ( 'NONE',  ( 1.000000000000000000, -0.000000000000000000, -0.000000000000000000 ) ) ;
#434 = CARTESIAN_POINT ( 'NONE',  ( 42.49999999999998579, 12.11403331821300533, 90.79316153445363113 ) ) ;
#435 = CARTESIAN_POINT ( 'NONE',  ( -10.00000000000000178, 19.67188320840964622, 26.15339366124404563 ) ) ;
#436 = CARTESIAN_POINT ( 'NONE',  ( -3.049447146744188153, 46.02418402111927520, 27.83478105833641791 ) ) ;
#437 = CARTESIAN_POINT ( 'NONE',  ( 24.65000000109246514, 20.00000000000000355, 83.29316153445364534 ) ) ;
#438 = VERTEX_POINT ( 'NONE', #3133 ) ;
#439 = VECTOR ( 'NONE', #5468, 1000.000000000000000 ) ;
#440 = CARTESIAN_POINT ( 'NONE',  ( -10.00000000000000355, 20.00000000000000355, -26.15339366124404563 ) ) ;
#441 = CONTEXT_DEPENDENT_SHAPE_REPRESENTATION ( #11941, #8818 ) ;
#442 = CARTESIAN_POINT ( 'NONE',  ( 3.974960981574284347, 46.94936902441865101, 24.68265737646872893 ) ) ;
#443 = CARTESIAN_POINT ( 'NONE',  ( 45.17500000054621978, 26.19570976099943493, 86.29171490190961435 ) ) ;
#444 = CARTESIAN_POINT ( 'NONE',  ( 25.07500000054622902, 26.19570976099943849, 86.29171490190961435 ) ) ;
#445 = CARTESIAN_POINT ( 'NONE',  ( 9.148278039838693587, 15.95559529756309836, 84.47248762917537590 ) ) ;
#446 = LINE ( 'NONE', #12178, #6529 ) ;
#447 = CARTESIAN_POINT ( 'NONE',  ( 0.000000000000000000, 139.9999999999999716, 0.000000000000000000 ) ) ;
#448 = CARTESIAN_POINT ( 'NONE',  ( 6.000000000000000000, 5.839897972853064445, -8.673617379884035472E-15 ) ) ;
#449 = CARTESIAN_POINT ( 'NONE',  ( 25.67500000054623044, 22.36655054427230027, 98.07665518445361386 ) ) ;
#450 = EDGE_LOOP ( 'NONE', ( #10994, #8391, #10133, #605, #8071 ) ) ;
#451 = CARTESIAN_POINT ( 'NONE',  ( 33.65000000109246514, 20.00000000000000355, 98.29316153445363113 ) ) ;
#452 = ORIENTED_EDGE ( 'NONE', *, *, #9229, .T. ) ;
#453 =( BOUNDED_CURVE ( )  B_SPLINE_CURVE ( 2, ( #5462, #5522, #10208, #12119, #6464, #693, #8432, #7289, #4309, #6522, #8188 ),
 .UNSPECIFIED., .F., .F. ) 
 B_SPLINE_CURVE_WITH_KNOTS ( ( 3, 2, 2, 2, 2, 3 ),
 ( 0.5333333333333333259, 0.5400000000000000355, 0.5466666666666666341, 0.5533333333333333437, 0.5600000000000000533, 0.5666666666666666519 ),
 .UNSPECIFIED. ) 
 CURVE ( )  GEOMETRIC_REPRESENTATION_ITEM ( )  RATIONAL_B_SPLINE_CURVE ( ( 1.000000000000000000, 0.9510565162951535312, 1.000000000000000000, 0.9510565162951535312, 1.000000000000000000, 0.9510565162951535312, 1.000000000000000000, 0.9510565162951535312, 1.000000000000000000, 0.9510565162951535312, 1.000000000000000000 ) ) 
 REPRESENTATION_ITEM ( '' )  );
#454 = DIRECTION ( 'NONE',  ( 1.000000000000000000, -0.000000000000000000, -0.000000000000000000 ) ) ;
#455 = EDGE_LOOP ( 'NONE', ( #6889, #11984, #9103, #7847, #1091 ) ) ;
#456 = EDGE_CURVE ( 'NONE', #3312, #5229, #7002, .T. ) ;
#457 =( NAMED_UNIT ( * ) SI_UNIT ( $, .STERADIAN. ) SOLID_ANGLE_UNIT ( ) );
#458 = CARTESIAN_POINT ( 'NONE',  ( 29.27500000054622475, 26.92701409722686634, 88.54243821818162985 ) ) ;
#459 = DIRECTION ( 'NONE',  ( 1.000000000000000000, 0.000000000000000000, 0.000000000000000000 ) ) ;
#460 = CARTESIAN_POINT ( 'NONE',  ( 47.07500000054621836, 26.19570976099943849, 86.29171490190961435 ) ) ;
#461 = CARTESIAN_POINT ( 'NONE',  ( 34.17500000054622689, 13.80429023900056507, 95.29460816699764791 ) ) ;
#462 = CARTESIAN_POINT ( 'NONE',  ( 38.19999999999998863, 15.59161060780645691, 96.86078899226572503 ) ) ;
#463 = CARTESIAN_POINT ( 'NONE',  ( 45.07500000054621836, 26.19570976099943493, 86.29171490190961435 ) ) ;
#464 = ORIENTED_EDGE ( 'NONE', *, *, #8533, .T. ) ;
#465 = CARTESIAN_POINT ( 'NONE',  ( 24.05000000109246372, 12.86707612778636012, 93.11078899226572503 ) ) ;
#466 = CARTESIAN_POINT ( 'NONE',  ( 32.00000000000000000, 6.167321280506070407E-16, -5.035999999999999588 ) ) ;
#467 = ORIENTED_EDGE ( 'NONE', *, *, #7068, .F. ) ;
#468 = CYLINDRICAL_SURFACE ( 'NONE', #9354, 5.000000000000000000 ) ;
#469 = ORIENTED_EDGE ( 'NONE', *, *, #2925, .T. ) ;
#470 = DIRECTION ( 'NONE',  ( -1.000000000000000000, -0.000000000000000000, -0.000000000000000000 ) ) ;
#471 = EDGE_CURVE ( 'NONE', #6633, #12230, #7168, .T. ) ;
#472 = FACE_BOUND ( 'NONE', #10780, .T. ) ;
#473 = FACE_OUTER_BOUND ( 'NONE', #1842, .T. ) ;
#474 = DIRECTION ( 'NONE',  ( 0.000000000000000000, 1.000000000000000000, 0.000000000000000000 ) ) ;
#475 = EDGE_CURVE ( 'NONE', #7179, #1407, #4444, .T. ) ;
#476 = CARTESIAN_POINT ( 'NONE',  ( 24.57500000054622902, 15.71886984736413773, 84.90069139318163138 ) ) ;
#477 = CARTESIAN_POINT ( 'NONE',  ( 26.97500000054622049, 22.36655054427230382, 83.50966788445364841 ) ) ;
#478 = AXIS2_PLACEMENT_3D ( 'NONE', #3709, #6569, #4544 ) ;
#479 = CARTESIAN_POINT ( 'NONE',  ( 2.282621191639543134, 29.74158684310808098, 27.90868772972744694 ) ) ;
#480 = LINE ( 'NONE', #419, #10100 ) ;
#481 = VERTEX_POINT ( 'NONE', #7503 ) ;
#482 = EDGE_CURVE ( 'NONE', #3396, #3276, #2495, .T. ) ;
#483 = CARTESIAN_POINT ( 'NONE',  ( 41.95000000109246230, 13.62011893735971135, 95.42841645007781892 ) ) ;
#484 = SURFACE_SIDE_STYLE ('',( #5430 ) ) ;
#485 = EDGE_LOOP ( 'NONE', ( #8313, #8253, #1494, #12322 ) ) ;
#486 = DIRECTION ( 'NONE',  ( -1.000000000000000000, -0.000000000000000000, -0.000000000000000000 ) ) ;
#487 = ORIENTED_EDGE ( 'NONE', *, *, #5188, .T. ) ;
#488 = CARTESIAN_POINT ( 'NONE',  ( 6.000000000000000000, 5.839897972853064445, -8.673617379884035472E-15 ) ) ;
#489 = CARTESIAN_POINT ( 'NONE',  ( 9.917674697986294419, 18.67684296126092747, -22.94866065126248600 ) ) ;
#490 = EDGE_CURVE ( 'NONE', #5212, #9224, #8457, .T. ) ;
#491 = DIRECTION ( 'NONE',  ( 0.000000000000000000, 0.000000000000000000, 1.000000000000000000 ) ) ;
#492 = CARTESIAN_POINT ( 'NONE',  ( 29.49999999999998934, 27.88596668178699645, 90.79316153445363113 ) ) ;
#493 = CARTESIAN_POINT ( 'NONE',  ( 0.000000000000000000, 67.00000000000000000, -28.00000000000000000 ) ) ;
#494 = CARTESIAN_POINT ( 'NONE',  ( 3.061616998149962604E-15, 10.00000000000000000, 25.00000000000000000 ) ) ;
#495 = FACE_OUTER_BOUND ( 'NONE', #10022, .T. ) ;
#496 = AXIS2_PLACEMENT_3D ( 'NONE', #5549, #658, #12392 ) ;
#497 = DIRECTION ( 'NONE',  ( 0.000000000000000000, 0.000000000000000000, -1.000000000000000000 ) ) ;
#498 = EDGE_CURVE ( 'NONE', #1359, #6574, #5547, .T. ) ;
#499 = CARTESIAN_POINT ( 'NONE',  ( 12.00000000000000178, 0.000000000000000000, 0.000000000000000000 ) ) ;
#500 = CARTESIAN_POINT ( 'NONE',  ( 2.612127725832936065, 29.65839247515747346, 24.86517017815632968 ) ) ;
#501 = AXIS2_PLACEMENT_3D ( 'NONE', #6674, #9361, #1670 ) ;
#502 = CARTESIAN_POINT ( 'NONE',  ( 6.955575927950914131E-22, 45.00000000000000711, -25.00000000000000000 ) ) ;
#503 = ORIENTED_EDGE ( 'NONE', *, *, #3690, .F. ) ;
#504 = CARTESIAN_POINT ( 'NONE',  ( -4.246666789336575931, 52.64435674096336015, 24.63684932116156645 ) ) ;
#505 = CARTESIAN_POINT ( 'NONE',  ( 12.59999999999999964, 0.000000000000000000, 0.000000000000000000 ) ) ;
#506 = VECTOR ( 'NONE', #2132, 1000.000000000000000 ) ;
#507 = CARTESIAN_POINT ( 'NONE',  ( 0.000000000000000000, 0.000000000000000000, 0.000000000000000000 ) ) ;
#508 = CARTESIAN_POINT ( 'NONE',  ( 43.07500000054622546, 24.28113015263587471, 84.90069139318163138 ) ) ;
#509 = CARTESIAN_POINT ( 'NONE',  ( 23.77500000054622831, 20.00000000000000355, 98.07665518445361386 ) ) ;
#510 = CARTESIAN_POINT ( 'NONE',  ( 10.00000000000000355, 20.00000000000000355, -22.91287847477919826 ) ) ;
#511 = DIRECTION ( 'NONE',  ( 0.000000000000000000, -1.000000000000000000, 0.000000000000000000 ) ) ;
#512 = CARTESIAN_POINT ( 'NONE',  ( 35.79999999999998295, 24.40838939219354842, 96.86078899226572503 ) ) ;
#513 = VERTEX_POINT ( 'NONE', #656 ) ;
#514 = CYLINDRICAL_SURFACE ( 'NONE', #5694, 7.499999999999992895 ) ;
#515 = ORIENTED_EDGE ( 'NONE', *, *, #5886, .T. ) ;
#516 = DIRECTION ( 'NONE',  ( 0.000000000000000000, 0.000000000000000000, -1.000000000000000000 ) ) ;
#517 = VECTOR ( 'NONE', #12407, 1000.000000000000000 ) ;
#518 = ORIENTED_EDGE ( 'NONE', *, *, #11469, .T. ) ;
#519 = CARTESIAN_POINT ( 'NONE',  ( 31.47500000054622404, 26.92701409722686634, 93.04388485072563242 ) ) ;
#520 = FACE_OUTER_BOUND ( 'NONE', #7436, .T. ) ;
#521 = CARTESIAN_POINT ( 'NONE',  ( 44.97500000054623115, 24.28113015263587471, 84.90069139318163138 ) ) ;
#522 = CARTESIAN_POINT ( 'NONE',  ( 33.17500000054622689, 26.19570976099943493, 86.29171490190961435 ) ) ;
#523 = CARTESIAN_POINT ( 'NONE',  ( 35.29999999999998295, 26.37988106264029398, 86.15790661882942914 ) ) ;
#524 = DIRECTION ( 'NONE',  ( 1.000000000000000000, 0.000000000000000000, 0.000000000000000000 ) ) ;
#525 = EDGE_CURVE ( 'NONE', #6104, #2798, #9416, .T. ) ;
#526 = CARTESIAN_POINT ( 'NONE',  ( 44.57500000054622546, 15.71886984736413773, 84.90069139318163138 ) ) ;
#527 = VERTEX_POINT ( 'NONE', #11245 ) ;
#528 = CARTESIAN_POINT ( 'NONE',  ( 25.05000000109246727, 27.13292387221364876, 88.47553407664153724 ) ) ;
#529 = CARTESIAN_POINT ( 'NONE',  ( -2.067585255946370548, 45.44456205236168245, 24.91481882275639848 ) ) ;
#530 = ORIENTED_EDGE ( 'NONE', *, *, #11604, .T. ) ;
#531 = CARTESIAN_POINT ( 'NONE',  ( -7.536943458953863306, 26.60426427458575205, 26.97071265772227378 ) ) ;
#532 = EDGE_LOOP ( 'NONE', ( #1378, #12293, #3921, #6914, #8507 ) ) ;
#533 = PLANE ( 'NONE',  #4547 ) ;
#534 = DIRECTION ( 'NONE',  ( -0.000000000000000000, -1.000000000000000000, -0.000000000000000000 ) ) ;
#535 = DIRECTION ( 'NONE',  ( 0.000000000000000000, 0.000000000000000000, 1.000000000000000000 ) ) ;
#536 = CARTESIAN_POINT ( 'NONE',  ( 27.49999999999999645, 20.00000000000000355, 189.9999999999999716 ) ) ;
#537 = CARTESIAN_POINT ( 'NONE',  ( 22.07500000054622546, 13.80429023900056507, 95.29460816699764791 ) ) ;
#538 = CARTESIAN_POINT ( 'NONE',  ( 24.87500000054622262, 20.00000000000000355, 83.50966788445364841 ) ) ;
#539 = CARTESIAN_POINT ( 'NONE',  ( 0.000000000000000000, 0.000000000000000000, 0.000000000000000000 ) ) ;
#540 = DIRECTION ( 'NONE',  ( -0.000000000000000000, -1.000000000000000000, -0.000000000000000000 ) ) ;
#541 = ORIENTED_EDGE ( 'NONE', *, *, #3157, .F. ) ;
#542 = CARTESIAN_POINT ( 'NONE',  ( 46.85000000109246798, 24.40838939219355197, 84.72553407664153724 ) ) ;
#543 = CARTESIAN_POINT ( 'NONE',  ( 4.339699721346885752, 52.50479725378321660, -24.62114839412567235 ) ) ;
#544 = ORIENTED_EDGE ( 'NONE', *, *, #6668, .F. ) ;
#545 = CARTESIAN_POINT ( 'NONE',  ( 29.85000000109246443, 15.59161060780645691, 96.86078899226572503 ) ) ;
#546 = ADVANCED_FACE ( 'NONE', ( #3566 ), #11187, .T. ) ;
#547 = ORIENTED_EDGE ( 'NONE', *, *, #2008, .F. ) ;
#548 = CARTESIAN_POINT ( 'NONE',  ( -2.620496854523448604, 10.32661740714168097, -24.87086379260451707 ) ) ;
#549 = CIRCLE ( 'NONE', #7628, 0.5999999999999998668 ) ;
#550 = CARTESIAN_POINT ( 'NONE',  ( 6.615773601782837687, 12.47291401044366310, -24.11353245396511014 ) ) ;
#551 = DIRECTION ( 'NONE',  ( 1.000000000000000000, 0.000000000000000000, 0.000000000000000000 ) ) ;
#552 = CARTESIAN_POINT ( 'NONE',  ( 12.59999999999999964, 0.000000000000000000, -6.600000000000003197 ) ) ;
#553 = DIRECTION ( 'NONE',  ( -0.000000000000000000, -0.000000000000000000, 1.000000000000000000 ) ) ;
#554 = CARTESIAN_POINT ( 'NONE',  ( 42.39999999999998437, 12.86707612778636012, 93.11078899226572503 ) ) ;
#555 = DIRECTION ( 'NONE',  ( 1.000000000000000000, 0.000000000000000000, 0.000000000000000000 ) ) ;
#556 = DIRECTION ( 'NONE',  ( -1.000000000000000000, -0.000000000000000000, 0.000000000000000000 ) ) ;
#557 = B_SPLINE_CURVE_WITH_KNOTS ( 'NONE', 3,
 ( #1543, #12013, #5417, #4214, #5170, #11953, #3317, #11555, #9592, #2864, #4581, #835, #5483, #4516, #5664, #7500, #4703, #1602, #10409, #6599, #900, #11308, #3622, #10532 ),
 .UNSPECIFIED., .F., .F.,
 ( 4, 2, 2, 2, 2, 2, 2, 2, 2, 2, 2, 4 ),
 ( 0.04728417969309388347, 0.04925452359716459005, 0.05023969554919995029, 0.05122486750123530358, 0.05221003945327065687, 0.05319521140530601017, 0.05516555530937670981, 0.05713589921344740252, 0.05910624311751810217, 0.06009141506955345546, 0.06107658702158880182, 0.06304693092565949453 ),
 .UNSPECIFIED. ) ;
#558 = CARTESIAN_POINT ( 'NONE',  ( -1.614380680224908104, 54.74360302825979119, 24.94967786989446878 ) ) ;
#559 = ORIENTED_EDGE ( 'NONE', *, *, #3887, .F. ) ;
#560 = CARTESIAN_POINT ( 'NONE',  ( 6.000000000000000000, -5.839897972853060892, 7.806255641895631925E-15 ) ) ;
#561 = EDGE_CURVE ( 'NONE', #8548, #852, #3785, .T. ) ;
#562 = CIRCLE ( 'NONE', #7444, 5.057500000000000107 ) ;
#563 = LINE ( 'NONE', #626, #4184 ) ;
#564 = CARTESIAN_POINT ( 'NONE',  ( 41.17500000054621978, 26.19570976099943493, 86.29171490190961435 ) ) ;
#565 = CARTESIAN_POINT ( 'NONE',  ( 29.97500000054622760, 15.71886984736413417, 96.68563167572563088 ) ) ;
#566 = CARTESIAN_POINT ( 'NONE',  ( 8.667493610547218452, 14.99723978859658935, 85.18566974208211207 ) ) ;
#567 = CARTESIAN_POINT ( 'NONE',  ( 0.000000000000000000, 18.00000000000000355, 169.9999999999999716 ) ) ;
#568 = CARTESIAN_POINT ( 'NONE',  ( 27.49999999999999645, 20.00000000000000355, 162.0000000000000000 ) ) ;
#569 = CARTESIAN_POINT ( 'NONE',  ( -6.999999999999999112, 34.57333724215600768, 127.4266627578445679 ) ) ;
#570 = ADVANCED_FACE ( 'NONE', ( #472, #5485 ), #8212, .T. ) ;
#571 = AXIS2_PLACEMENT_3D ( 'NONE', #4157, #3457, #6315 ) ;
#572 = ORIENTED_EDGE ( 'NONE', *, *, #5822, .T. ) ;
#573 = LINE ( 'NONE', #5584, #10338 ) ;
#574 = VERTEX_POINT ( 'NONE', #3382 ) ;
#575 = DIRECTION ( 'NONE',  ( -0.000000000000000000, -1.000000000000000000, -0.000000000000000000 ) ) ;
#576 = DIRECTION ( 'NONE',  ( 0.000000000000000000, 0.000000000000000000, 1.000000000000000000 ) ) ;
#577 = AXIS2_PLACEMENT_3D ( 'NONE', #5068, #2970, #6082 ) ;
#578 = B_SPLINE_CURVE_WITH_KNOTS ( 'NONE', 3,
 ( #2023, #1152, #7096, #9774, #1084, #4949, #8813, #197, #3991, #11740, #6907, #6028, #7933, #9902, #9201, #5330, #12117, #12239, #6399, #6279, #8248, #1402, #8185, #2462, #3420, #510 ),
 .UNSPECIFIED., .F., .F.,
 ( 4, 2, 2, 2, 2, 2, 2, 2, 2, 2, 2, 2, 4 ),
 ( 0.03159890529972236156, 0.03258580175252957789, 0.03357269820533679422, 0.03554649111095121994, 0.03653338756375844321, 0.03752028401656565260, 0.03949407692218008525, 0.04146786982779451791, 0.04245476628060172730, 0.04344166273340894363, 0.04541545563902336935, 0.04640235209183058568, 0.04738924854463780201 ),
 .UNSPECIFIED. ) ;
#579 = CARTESIAN_POINT ( 'NONE',  ( 31.87500000054622262, 20.00000000000000355, 98.07665518445361386 ) ) ;
#580 = CARTESIAN_POINT ( 'NONE',  ( -4.339864767223333253, 52.50448352687625686, -27.66223537364948015 ) ) ;
#581 = CARTESIAN_POINT ( 'NONE',  ( 45.37500000054622973, 26.92701409722686634, 93.04388485072563242 ) ) ;
#582 = CARTESIAN_POINT ( 'NONE',  ( 31.47500000054622404, 26.92701409722686634, 93.04388485072563242 ) ) ;
#583 = CARTESIAN_POINT ( 'NONE',  ( 33.19999999999998863, 24.40838939219355197, 84.72553407664153724 ) ) ;
#584 = CARTESIAN_POINT ( 'NONE',  ( 9.916835782772588814, 21.32911185711201796, 22.94902338049798374 ) ) ;
#585 = CARTESIAN_POINT ( 'NONE',  ( 40.87500000054623683, 22.36655054427230382, 83.50966788445364841 ) ) ;
#586 = ORIENTED_EDGE ( 'NONE', *, *, #10084, .T. ) ;
#587 = CARTESIAN_POINT ( 'NONE',  ( 46.07500000054623257, 13.80429023900056507, 95.29460816699764791 ) ) ;
#588 = LINE ( 'NONE', #9035, #618 ) ;
#589 = VERTEX_POINT ( 'NONE', #2552 ) ;
#590 = AXIS2_PLACEMENT_3D ( 'NONE', #448, #12242, #3603 ) ;
#591 = CARTESIAN_POINT ( 'NONE',  ( -5.033433411003701785, 28.66518080936452861, 27.54934970082421941 ) ) ;
#592 = ORIENTED_EDGE ( 'NONE', *, *, #4345, .F. ) ;
#593 = VECTOR ( 'NONE', #11463, 1000.000000000000000 ) ;
#594 = DIRECTION ( 'NONE',  ( 0.000000000000000000, -0.5000000000000009992, -0.8660254037844380415 ) ) ;
#595 = CIRCLE ( 'NONE', #1008, 10.00000000000000355 ) ;
#596 = DIRECTION ( 'NONE',  ( -1.000000000000000000, 0.000000000000000000, 0.000000000000000000 ) ) ;
#597 = LINE ( 'NONE', #3505, #11293 ) ;
#598 = EDGE_CURVE ( 'NONE', #3966, #5275, #11124, .T. ) ;
#599 = CARTESIAN_POINT ( 'NONE',  ( 32.05000000109247082, 12.86707612778636012, 93.11078899226572503 ) ) ;
#600 = CARTESIAN_POINT ( 'NONE',  ( 21.47500000054622760, 26.19570976099943493, 95.29460816699764791 ) ) ;
#601 = CARTESIAN_POINT ( 'NONE',  ( 27.37500000054622262, 27.65831843345427998, 90.79316153445363113 ) ) ;
#602 = DIRECTION ( 'NONE',  ( 0.000000000000000000, 0.000000000000000000, 1.000000000000000000 ) ) ;
#603 = AXIS2_PLACEMENT_3D ( 'NONE', #10554, #4789, #8655 ) ;
#604 = CARTESIAN_POINT ( 'NONE',  ( -4.493559251511619834, 47.78304274923282691, 24.59317321405577772 ) ) ;
#605 = ORIENTED_EDGE ( 'NONE', *, *, #1416, .T. ) ;
#606 = CARTESIAN_POINT ( 'NONE',  ( 42.25000000109246656, 12.86707612778636012, 88.47553407664152303 ) ) ;
#607 = EDGE_LOOP ( 'NONE', ( #9363, #7842, #4031, #12501, #7877, #12339 ) ) ;
#608 = CARTESIAN_POINT ( 'NONE',  ( -2.000000000000015543, 20.00000000000000355, 90.79316153445363113 ) ) ;
#609 = EDGE_LOOP ( 'NONE', ( #745, #2763, #10847, #363, #6595 ) ) ;
#610 = CARTESIAN_POINT ( 'NONE',  ( -7.514688383768903357, 13.39426057884744026, -23.84485093628785535 ) ) ;
#611 = CARTESIAN_POINT ( 'NONE',  ( 2.620611987601386250, 10.32688167823381953, -24.87076294850758984 ) ) ;
#612 = EDGE_CURVE ( 'NONE', #2987, #6725, #1484, .T. ) ;
#613 = FACE_OUTER_BOUND ( 'NONE', #1110, .T. ) ;
#614 = FILL_AREA_STYLE ('',( #3283 ) ) ;
#615 = ADVANCED_FACE ( 'NONE', ( #3449 ), #7315, .F. ) ;
#616 = CARTESIAN_POINT ( 'NONE',  ( 5.000000000000000888, 50.00000000000000000, -20.39607805437114152 ) ) ;
#617 = DIRECTION ( 'NONE',  ( -1.000000000000000000, 0.000000000000000000, -0.000000000000000000 ) ) ;
#618 = VECTOR ( 'NONE', #347, 1000.000000000000000 ) ;
#619 = CARTESIAN_POINT ( 'NONE',  ( 12.59999999999999964, 0.000000000000000000, 0.000000000000000000 ) ) ;
#620 = CARTESIAN_POINT ( 'NONE',  ( 31.03600000000003689, 0.000000000000000000, 0.000000000000000000 ) ) ;
#621 = CARTESIAN_POINT ( 'NONE',  ( 4.444397983376138228, 28.96407317687630822, 24.60352964329958070 ) ) ;
#622 = CARTESIAN_POINT ( 'NONE',  ( -4.839306774598123084, 51.30008082132634684, 24.52723862394605092 ) ) ;
#623 = EDGE_LOOP ( 'NONE', ( #2309, #2368, #2131 ) ) ;
#624 = CIRCLE ( 'NONE', #3462, 7.500000000000000000 ) ;
#625 = DIRECTION ( 'NONE',  ( 1.000000000000000000, 0.000000000000000000, 0.000000000000000000 ) ) ;
#626 = CARTESIAN_POINT ( 'NONE',  ( -2.000000000000015543, 20.00000000000000355, 98.29316153445363113 ) ) ;
#627 = CARTESIAN_POINT ( 'NONE',  ( 36.07500000054622546, 15.71886984736413417, 96.68563167572563088 ) ) ;
#628 = CARTESIAN_POINT ( 'NONE',  ( 25.67500000054623044, 22.36655054427230027, 98.07665518445361386 ) ) ;
#629 = CARTESIAN_POINT ( 'NONE',  ( 7.061248332739769040, 12.91833545835538288, 88.31103790290751476 ) ) ;
#630 = CARTESIAN_POINT ( 'NONE',  ( 4.967390183827647299, 49.34301876381886132, 24.50161767623307441 ) ) ;
#631 = DIRECTION ( 'NONE',  ( -0.000000000000000000, -0.000000000000000000, 1.000000000000000000 ) ) ;
#632 = DIRECTION ( 'NONE',  ( 0.000000000000000000, 0.000000000000000000, -1.000000000000000000 ) ) ;
#633 = EDGE_LOOP ( 'NONE', ( #366, #4722, #9019, #2561 ) ) ;
#634 = AXIS2_PLACEMENT_3D ( 'NONE', #11656, #12414, #9926 ) ;
#635 = ADVANCED_FACE ( 'NONE', ( #4459 ), #8338, .T. ) ;
#636 = DIRECTION ( 'NONE',  ( 0.000000000000000000, 0.000000000000000000, -1.000000000000000000 ) ) ;
#637 = VERTEX_POINT ( 'NONE', #5729 ) ;
#638 = FACE_BOUND ( 'NONE', #9288, .T. ) ;
#639 = ADVANCED_FACE ( 'NONE', ( #11621 ), #4645, .F. ) ;
#640 = EDGE_CURVE ( 'NONE', #4818, #9118, #196, .T. ) ;
#641 = CARTESIAN_POINT ( 'NONE',  ( 32.57500000054622546, 13.80429023900056684, 86.29171490190961435 ) ) ;
#642 = CARTESIAN_POINT ( 'NONE',  ( 27.35000000109246443, 26.37988106264029398, 95.42841645007781892 ) ) ;
#643 = CARTESIAN_POINT ( 'NONE',  ( 47.77500000054622831, 20.00000000000000355, 98.07665518445361386 ) ) ;
#644 = CARTESIAN_POINT ( 'NONE',  ( 35.67500000054622689, 24.28113015263587116, 96.68563167572563088 ) ) ;
#645 = CARTESIAN_POINT ( 'NONE',  ( 38.49999999999999289, 12.11403331821300533, 90.79316153445363113 ) ) ;
#646 = CARTESIAN_POINT ( 'NONE',  ( -1.322110193236855746, 29.91777919888772885, 20.96095187701988394 ) ) ;
#647 = EDGE_CURVE ( 'NONE', #5544, #10865, #2369, .T. ) ;
#648 = CARTESIAN_POINT ( 'NONE',  ( 37.37500000054622973, 26.92701409722686634, 93.04388485072563242 ) ) ;
#649 = ORIENTED_EDGE ( 'NONE', *, *, #2660, .F. ) ;
#650 = CARTESIAN_POINT ( 'NONE',  ( 48.17500000054623399, 13.07298590277314254, 93.04388485072563242 ) ) ;
#651 = CARTESIAN_POINT ( 'NONE',  ( 0.000000000000000000, 0.000000000000000000, -25.00000000000000000 ) ) ;
#652 = VERTEX_POINT ( 'NONE', #11434 ) ;
#653 = CARTESIAN_POINT ( 'NONE',  ( 3.561025220032636440, 10.64985055133391079, 20.69813086000296209 ) ) ;
#654 = ORIENTED_EDGE ( 'NONE', *, *, #179, .T. ) ;
#655 = CARTESIAN_POINT ( 'NONE',  ( 41.65000000109246514, 20.00000000000000355, 98.29316153445363113 ) ) ;
#656 = CARTESIAN_POINT ( 'NONE',  ( 37.99999999999999289, 20.00000000000000355, 98.29316153445363113 ) ) ;
#657 = CYLINDRICAL_SURFACE ( 'NONE', #974, 5.999999999999999112 ) ;
#658 = DIRECTION ( 'NONE',  ( 1.000000000000000000, -0.000000000000000000, -0.000000000000000000 ) ) ;
#659 = CARTESIAN_POINT ( 'NONE',  ( 23.27500000054622120, 27.65831843345427998, 90.79316153445363113 ) ) ;
#660 = CARTESIAN_POINT ( 'NONE',  ( 25.57500000054621836, 26.19570976099943493, 95.29460816699764791 ) ) ;
#661 = FACE_OUTER_BOUND ( 'NONE', #1808, .T. ) ;
#662 =( BOUNDED_CURVE ( )  B_SPLINE_CURVE ( 2, ( #4095, #9942, #12155, #4408, #11197, #8286, #1618, #7453, #545, #5432, #11137 ),
 .UNSPECIFIED., .F., .F. ) 
 B_SPLINE_CURVE_WITH_KNOTS ( ( 3, 2, 2, 2, 2, 3 ),
 ( 0.6333333333333333037, 0.6400000000000000133, 0.6466666666666666119, 0.6533333333333333215, 0.6600000000000000311, 0.6666666666666666297 ),
 .UNSPECIFIED. ) 
 CURVE ( )  GEOMETRIC_REPRESENTATION_ITEM ( )  RATIONAL_B_SPLINE_CURVE ( ( 1.000000000000000000, 0.9510565162951535312, 1.000000000000000000, 0.9510565162951535312, 1.000000000000000000, 0.9510565162951535312, 1.000000000000000000, 0.9510565162951535312, 1.000000000000000000, 0.9510565162951535312, 1.000000000000000000 ) ) 
 REPRESENTATION_ITEM ( '' )  );
#663 = CARTESIAN_POINT ( 'NONE',  ( 44.89999999999998437, 17.56310227825322912, 83.29316153445361692 ) ) ;
#664 = ORIENTED_EDGE ( 'NONE', *, *, #6410, .F. ) ;
#665 = CARTESIAN_POINT ( 'NONE',  ( 39.15000000109246514, 27.88596668178699645, 90.79316153445363113 ) ) ;
#666 =( NAMED_UNIT ( * ) SI_UNIT ( $, .STERADIAN. ) SOLID_ANGLE_UNIT ( ) );
#667 = VERTEX_POINT ( 'NONE', #3941 ) ;
#668 = DIRECTION ( 'NONE',  ( 1.000000000000000000, -0.000000000000000000, -0.000000000000000000 ) ) ;
#669 = ORIENTED_EDGE ( 'NONE', *, *, #11328, .T. ) ;
#670 = CARTESIAN_POINT ( 'NONE',  ( -3.245616027290198602, 10.51897860477085622, -24.79588311023535852 ) ) ;
#671 = CARTESIAN_POINT ( 'NONE',  ( 9.917815328463536417, 18.67816480429018711, -18.51049262088216807 ) ) ;
#672 = CYLINDRICAL_SURFACE ( 'NONE', #85, 8.000000000000000000 ) ;
#673 = AXIS2_PLACEMENT_3D ( 'NONE', #4631, #7426, #822 ) ;
#674 = CARTESIAN_POINT ( 'NONE',  ( 6.000000000000000000, -5.839897972853060892, 7.806255641895631925E-15 ) ) ;
#675 = DIRECTION ( 'NONE',  ( 1.000000000000000000, -0.000000000000000000, -0.000000000000000000 ) ) ;
#676 = DIRECTION ( 'NONE',  ( 0.000000000000000000, 0.000000000000000000, 1.000000000000000000 ) ) ;
#677 = CARTESIAN_POINT ( 'NONE',  ( 0.000000000000000000, 139.9999999999999716, 0.000000000000000000 ) ) ;
#678 = CARTESIAN_POINT ( 'NONE',  ( 29.87500000054622618, 17.63344945572769973, 98.07665518445361386 ) ) ;
#679 = ADVANCED_FACE ( 'NONE', ( #6727, #838 ), #7692, .T. ) ;
#680 = LINE ( 'NONE', #5511, #2953 ) ;
#681 = PLANE ( 'NONE',  #9133 ) ;
#682 = ORIENTED_EDGE ( 'NONE', *, *, #2491, .T. ) ;
#683 = AXIS2_PLACEMENT_3D ( 'NONE', #3608, #3550, #2786 ) ;
#684 = CARTESIAN_POINT ( 'NONE',  ( 12.59999999999999964, 0.000000000000000000, 5.999999999999999112 ) ) ;
#685 = LINE ( 'NONE', #8552, #3386 ) ;
#686 = CARTESIAN_POINT ( 'NONE',  ( 34.97500000054623115, 24.28113015263587471, 84.90069139318163138 ) ) ;
#687 = CARTESIAN_POINT ( 'NONE',  ( 38.57500000054622546, 13.80429023900056684, 86.29171490190961435 ) ) ;
#688 = CONICAL_SURFACE ( 'NONE', #7982, 4.057500000000000107, 1.047197551196593857 ) ;
#689 = CARTESIAN_POINT ( 'NONE',  ( 26.77500000054622831, 20.00000000000000355, 83.50966788445364841 ) ) ;
#690 = DIRECTION ( 'NONE',  ( 0.000000000000000000, 0.000000000000000000, 1.000000000000000000 ) ) ;
#691 = DIRECTION ( 'NONE',  ( 0.000000000000000000, -0.5000000000000012212, -0.8660254037844380415 ) ) ;
#692 = CIRCLE ( 'NONE', #8795, 7.499999999999992895 ) ;
#693 = CARTESIAN_POINT ( 'NONE',  ( 33.49999999999998579, 27.88596668178699645, 90.79316153445363113 ) ) ;
#694 = CARTESIAN_POINT ( 'NONE',  ( 27.49999999999999645, 20.00000000000000355, 189.9999999999999716 ) ) ;
#695 = ORIENTED_EDGE ( 'NONE', *, *, #9724, .T. ) ;
#696 = CARTESIAN_POINT ( 'NONE',  ( 27.49999999999999645, 20.00000000000000355, 170.0000119999999697 ) ) ;
#697 = EDGE_CURVE ( 'NONE', #1603, #438, #5063, .T. ) ;
#698 = PRODUCT_CONTEXT ( 'NONE', #3666, 'mechanical' ) ;
#699 = VECTOR ( 'NONE', #7974, 1000.000000000000000 ) ;
#700 = CARTESIAN_POINT ( 'NONE',  ( 27.47500000054622404, 26.92701409722686634, 93.04388485072563242 ) ) ;
#701 = CARTESIAN_POINT ( 'NONE',  ( 26.75000000109246656, 22.43689772174683128, 83.29316153445365956 ) ) ;
#702 = CARTESIAN_POINT ( 'NONE',  ( 49.17500000054622689, 26.92701409722686634, 88.54243821818162985 ) ) ;
#703 = CARTESIAN_POINT ( 'NONE',  ( 32.97500000054621694, 22.36655054427230382, 83.50966788445364841 ) ) ;
#704 = CARTESIAN_POINT ( 'NONE',  ( 32.19999999999999574, 15.59161060780645691, 96.86078899226572503 ) ) ;
#705 = CARTESIAN_POINT ( 'NONE',  ( -5.310537848405668448, 28.47956428665436235, 20.31934704339811049 ) ) ;
#706 = CARTESIAN_POINT ( 'NONE',  ( 36.87500000054622973, 22.36655054427230382, 83.50966788445364841 ) ) ;
#707 = VERTEX_POINT ( 'NONE', #11558 ) ;
#708 =( GEOMETRIC_REPRESENTATION_CONTEXT ( 3 ) GLOBAL_UNCERTAINTY_ASSIGNED_CONTEXT ( ( #3862 ) ) GLOBAL_UNIT_ASSIGNED_CONTEXT ( ( #7814, #3430, #457 ) ) REPRESENTATION_CONTEXT ( 'NONE', 'WORKASPACE' ) );
#709 = AXIS2_PLACEMENT_3D ( 'NONE', #12100, #12221, #7145 ) ;
#710 = CARTESIAN_POINT ( 'NONE',  ( 47.87500000054622973, 17.63344945572769973, 98.07665518445361386 ) ) ;
#711 = LINE ( 'NONE', #651, #11144 ) ;
#712 = ORIENTED_EDGE ( 'NONE', *, *, #2572, .T. ) ;
#713 = ADVANCED_FACE ( 'NONE', ( #12510 ), #10472, .F. ) ;
#714 = DIRECTION ( 'NONE',  ( -0.000000000000000000, -1.000000000000000000, -0.000000000000000000 ) ) ;
#715 = ORIENTED_EDGE ( 'NONE', *, *, #4970, .T. ) ;
#716 = CARTESIAN_POINT ( 'NONE',  ( 8.484924050289805564, 25.30202893790023921, -23.51686326738786192 ) ) ;
#717 = CARTESIAN_POINT ( 'NONE',  ( 10.00000000000000355, 20.00000000000000355, 26.15339366124404563 ) ) ;
#718 = DIRECTION ( 'NONE',  ( 0.000000000000000000, 0.000000000000000000, -1.000000000000000000 ) ) ;
#719 = DIRECTION ( 'NONE',  ( 0.000000000000000000, 0.000000000000000000, -1.000000000000000000 ) ) ;
#720 = EDGE_CURVE ( 'NONE', #5074, #10184, #8439, .T. ) ;
#721 = CARTESIAN_POINT ( 'NONE',  ( 23.57500000054622902, 24.28113015263587116, 96.68563167572563088 ) ) ;
#722 = CARTESIAN_POINT ( 'NONE',  ( 49.29999999999998295, 26.37988106264029398, 86.15790661882942914 ) ) ;
#723 = CARTESIAN_POINT ( 'NONE',  ( -3.554546826686217020, 29.35267307038308360, -24.74790415999775917 ) ) ;
#724 = VERTEX_POINT ( 'NONE', #9662 ) ;
#725 = AXIS2_PLACEMENT_3D ( 'NONE', #3592, #2392, #3529 ) ;
#726 = CARTESIAN_POINT ( 'NONE',  ( 34.95000000109246940, 26.37988106264029398, 86.15790661882942914 ) ) ;
#727 = ORIENTED_EDGE ( 'NONE', *, *, #7144, .F. ) ;
#728 = FILL_AREA_STYLE_COLOUR ( '', #6260 ) ;
#729 = EDGE_CURVE ( 'NONE', #3966, #852, #8760, .T. ) ;
#730 = VERTEX_POINT ( 'NONE', #1726 ) ;
#731 = CARTESIAN_POINT ( 'NONE',  ( 2.218782135151963431, 54.49261812855775844, 20.88465242318871873 ) ) ;
#732 = CARTESIAN_POINT ( 'NONE',  ( 5.340684424226280325E-17, 55.00000000000000000, -25.00000000000000000 ) ) ;
#733 = CARTESIAN_POINT ( 'NONE',  ( 6.000000000000000000, 0.000000000000000000, 5.057500000000000107 ) ) ;
#734 =( BOUNDED_CURVE ( )  B_SPLINE_CURVE ( 2, ( #10941, #6123, #9991, #1304, #5174, #9043, #7835, #11704, #354, #163, #11643 ),
 .UNSPECIFIED., .F., .F. ) 
 B_SPLINE_CURVE_WITH_KNOTS ( ( 3, 2, 2, 2, 2, 3 ),
 ( 0.03333333333333336063, 0.04000000000000003553, 0.04666666666666670349, 0.05333333333333337839, 0.06000000000000005329, 0.06666666666666672125 ),
 .UNSPECIFIED. ) 
 CURVE ( )  GEOMETRIC_REPRESENTATION_ITEM ( )  RATIONAL_B_SPLINE_CURVE ( ( 0.9999999999999998890, 0.9510565162951537532, 1.000000000000000000, 0.9510565162951535312, 1.000000000000000000, 0.9510565162951535312, 1.000000000000000000, 0.9510565162951535312, 1.000000000000000000, 0.9510565162951530871, 1.000000000000000444 ) ) 
 REPRESENTATION_ITEM ( '' )  );
#735 = FACE_OUTER_BOUND ( 'NONE', #2724, .T. ) ;
#736 = CARTESIAN_POINT ( 'NONE',  ( 6.000000000000000000, 2.919948986426526005, -5.057500000000003659 ) ) ;
#737 = EDGE_CURVE ( 'NONE', #5428, #8208, #5928, .T. ) ;
#738 = LINE ( 'NONE', #9227, #506 ) ;
#739 = CARTESIAN_POINT ( 'NONE',  ( 48.15000000109246514, 12.11403331821300533, 90.79316153445363113 ) ) ;
#740 = CARTESIAN_POINT ( 'NONE',  ( 20.37500000054622618, 13.07298590277314432, 88.54243821818161564 ) ) ;
#741 = CARTESIAN_POINT ( 'NONE',  ( 9.657343816332662811, 22.61594140643868300, 23.05962942824199757 ) ) ;
#742 = CARTESIAN_POINT ( 'NONE',  ( 47.55000000109247082, 22.43689772174681707, 98.29316153445361692 ) ) ;
#743 = ORIENTED_EDGE ( 'NONE', *, *, #1458, .F. ) ;
#744 = AXIS2_PLACEMENT_3D ( 'NONE', #12233, #8244, #11213 ) ;
#745 = ORIENTED_EDGE ( 'NONE', *, *, #3310, .F. ) ;
#746 = CARTESIAN_POINT ( 'NONE',  ( -3.255620798467798060, 29.46102596484070446, -20.74857864660710405 ) ) ;
#747 = EDGE_CURVE ( 'NONE', #3111, #7940, #4337, .T. ) ;
#748 = DIRECTION ( 'NONE',  ( 0.000000000000000000, 1.000000000000000000, 0.000000000000000000 ) ) ;
#749 = CARTESIAN_POINT ( 'NONE',  ( 36.77500000054622831, 17.63344945572770328, 83.50966788445364841 ) ) ;
#750 = COLOUR_RGB ( '',0.7921568627450980005, 0.8196078431372548767, 0.9333333333333333481 ) ;
#751 = CARTESIAN_POINT ( 'NONE',  ( 22.37500000054622973, 13.07298590277314432, 88.54243821818161564 ) ) ;
#752 = LINE ( 'NONE', #10574, #10296 ) ;
#753 = CARTESIAN_POINT ( 'NONE',  ( 1.298299055536097368, 45.16027954822755675, 24.96835849755778014 ) ) ;
#754 = DIRECTION ( 'NONE',  ( -0.000000000000000000, -0.000000000000000000, -1.000000000000000000 ) ) ;
#755 = DIRECTION ( 'NONE',  ( 0.000000000000000000, 1.000000000000000000, 0.000000000000000000 ) ) ;
#756 = ADVANCED_FACE ( 'NONE', ( #9914, #7944 ), #2238, .T. ) ;
#757 = DIRECTION ( 'NONE',  ( 0.000000000000000000, 0.4999999999999987232, -0.8660254037844393737 ) ) ;
#758 = ORIENTED_EDGE ( 'NONE', *, *, #7126, .F. ) ;
#759 = DIRECTION ( 'NONE',  ( 0.000000000000000000, 1.000000000000000000, -1.295896757998781374E-15 ) ) ;
#760 = DIRECTION ( 'NONE',  ( 1.000000000000000000, 0.000000000000000000, 0.000000000000000000 ) ) ;
#761 = CARTESIAN_POINT ( 'NONE',  ( 39.27500000054622120, 27.65831843345427998, 90.79316153445363113 ) ) ;
#762 = CARTESIAN_POINT ( 'NONE',  ( 28.47500000054622404, 13.07298590277314432, 88.54243821818161564 ) ) ;
#763 = CARTESIAN_POINT ( 'NONE',  ( 29.49999999999998934, 27.88596668178699645, 90.79316153445363113 ) ) ;
#764 = EDGE_CURVE ( 'NONE', #9148, #8716, #2992, .T. ) ;
#765 = CARTESIAN_POINT ( 'NONE',  ( 5.000000000000000000, 4.685197434473814759, -5.637851296924623057E-15 ) ) ;
#766 = CARTESIAN_POINT ( 'NONE',  ( 39.37500000054622973, 26.92701409722686634, 93.04388485072563242 ) ) ;
#767 = ORIENTED_EDGE ( 'NONE', *, *, #1303, .T. ) ;
#768 = CARTESIAN_POINT ( 'NONE',  ( 21.55000000109246017, 22.43689772174679575, 98.29316153445363113 ) ) ;
#769 = CARTESIAN_POINT ( 'NONE',  ( -5.000000000000000000, 50.00000000000000000, -20.39607805437114152 ) ) ;
#770 = ORIENTED_EDGE ( 'NONE', *, *, #11974, .F. ) ;
#771 = PRODUCT_DEFINITION ( 'UNKNOWN', '', #6364, #5110 ) ;
#772 = CARTESIAN_POINT ( 'NONE',  ( 9.932934464065827029, 18.66923383145512005, 18.50293221336126237 ) ) ;
#773 = EDGE_LOOP ( 'NONE', ( #9656, #898, #9194, #268, #11639 ) ) ;
#774 = AXIS2_PLACEMENT_3D ( 'NONE', #1994, #5875, #10884 ) ;
#775 = CARTESIAN_POINT ( 'NONE',  ( -0.6569842770428546697, 54.96739046863824996, -24.99342020365237360 ) ) ;
#776 = DIRECTION ( 'NONE',  ( -1.000000000000000000, -0.000000000000000000, -0.000000000000000000 ) ) ;
#777 =( BOUNDED_CURVE ( )  B_SPLINE_CURVE ( 2, ( #7759, #3949, #2936, #6801, #10668, #1977, #6866, #10730, #2042, #8250, #5333 ),
 .UNSPECIFIED., .F., .F. ) 
 B_SPLINE_CURVE_WITH_KNOTS ( ( 3, 2, 2, 2, 2, 3 ),
 ( 0.2999999999999999889, 0.3066666666666666430, 0.3133333333333333526, 0.3200000000000000622, 0.3266666666666667163, 0.3333333333333333703 ),
 .UNSPECIFIED. ) 
 CURVE ( )  GEOMETRIC_REPRESENTATION_ITEM ( )  RATIONAL_B_SPLINE_CURVE ( ( 1.000000000000000000, 0.9510565162951535312, 1.000000000000000000, 0.9510565162951535312, 1.000000000000000000, 0.9510565162951535312, 1.000000000000000000, 0.9510565162951535312, 1.000000000000000000, 0.9510565162951530871, 1.000000000000000444 ) ) 
 REPRESENTATION_ITEM ( '' )  );
#778 = PRESENTATION_LAYER_ASSIGNMENT (  '', '', ( #6254 ) ) ;
#779 = CARTESIAN_POINT ( 'NONE',  ( 42.57500000054622546, 13.80429023900056684, 86.29171490190961435 ) ) ;
#780 = CARTESIAN_POINT ( 'NONE',  ( 3.429011037612589276E-15, 67.00000000000000000, 28.00000000000000000 ) ) ;
#781 = CARTESIAN_POINT ( 'NONE',  ( 45.67500000054621978, 24.28113015263587116, 96.68563167572563088 ) ) ;
#782 = CARTESIAN_POINT ( 'NONE',  ( 47.79999999999999005, 24.40838939219354842, 96.86078899226572503 ) ) ;
#783 = DIRECTION ( 'NONE',  ( 1.000000000000000000, 0.000000000000000000, 0.000000000000000000 ) ) ;
#784 = CARTESIAN_POINT ( 'NONE',  ( 39.45000000109246230, 24.40838939219354842, 96.86078899226572503 ) ) ;
#785 = AXIS2_PLACEMENT_3D ( 'NONE', #3854, #7731, #7665 ) ;
#786 = EDGE_LOOP ( 'NONE', ( #8143, #3316, #7200, #5938 ) ) ;
#787 = CARTESIAN_POINT ( 'NONE',  ( 37.95000000109246940, 13.62011893735971135, 95.42841645007781892 ) ) ;
#788 = LINE ( 'NONE', #11445, #53 ) ;
#789 = ORIENTED_EDGE ( 'NONE', *, *, #9389, .F. ) ;
#790 = CARTESIAN_POINT ( 'NONE',  ( 49.99999999999998579, 0.000000000000000000, 69.99999999999998579 ) ) ;
#791 = EDGE_CURVE ( 'NONE', #2265, #6417, #2144, .T. ) ;
#792 = ORIENTED_EDGE ( 'NONE', *, *, #1167, .F. ) ;
#793 = CARTESIAN_POINT ( 'NONE',  ( -2.000000000000015543, 20.00000000000000355, 90.79316153445363113 ) ) ;
#794 = CARTESIAN_POINT ( 'NONE',  ( 6.113716319958878209, 12.07992478634019662, -20.09207169644096780 ) ) ;
#795 = CARTESIAN_POINT ( 'NONE',  ( -10.00000000000000178, 20.32878730486446273, 22.91287847477919826 ) ) ;
#796 = EDGE_CURVE ( 'NONE', #11194, #12230, #5974, .T. ) ;
#797 = ADVANCED_FACE ( 'NONE', ( #11879 ), #3185, .F. ) ;
#798 = CLOSED_SHELL ( 'NONE', ( #7102, #11031, #3425, #12222, #9856, #7107, #9235, #2450, #570, #3722, #6454, #5883, #7818, #6592, #5655, #2029, #10833, #3408, #1229, #5066, #2806, #9157, #3585, #11147, #6385, #11013, #2555 ) ) ;
#799 = LINE ( 'NONE', #9557, #1526 ) ;
#800 = DIRECTION ( 'NONE',  ( 1.000000000000000000, 0.000000000000000000, 0.000000000000000000 ) ) ;
#801 = VERTEX_POINT ( 'NONE', #9024 ) ;
#802 = CARTESIAN_POINT ( 'NONE',  ( -50.00000000000001421, 18.00000000000000355, 188.4007504869563263 ) ) ;
#803 = FACE_OUTER_BOUND ( 'NONE', #8940, .T. ) ;
#804 = CARTESIAN_POINT ( 'NONE',  ( 48.37500000054621552, 12.34168156654572535, 90.79316153445363113 ) ) ;
#805 = LINE ( 'NONE', #4675, #5389 ) ;
#806 = ORIENTED_EDGE ( 'NONE', *, *, #2258, .F. ) ;
#807 = ORIENTED_EDGE ( 'NONE', *, *, #2968, .T. ) ;
#808 = CARTESIAN_POINT ( 'NONE',  ( 1.342157722727130131E-15, 30.00000000000002132, -21.00000000000000355 ) ) ;
#809 = AXIS2_PLACEMENT_3D ( 'NONE', #9471, #11429, #1660 ) ;
#810 = FACE_OUTER_BOUND ( 'NONE', #773, .T. ) ;
#811 = CARTESIAN_POINT ( 'NONE',  ( 19.77500000054622831, 20.00000000000000355, 98.07665518445361386 ) ) ;
#812 = PLANE ( 'NONE',  #785 ) ;
#813 = LINE ( 'NONE', #7161, #2327 ) ;
#814 = DIRECTION ( 'NONE',  ( -1.000000000000000000, -0.000000000000000000, -0.000000000000000000 ) ) ;
#815 = CARTESIAN_POINT ( 'NONE',  ( 1.295138726946435170, 45.15964000046352567, 27.97186371880082234 ) ) ;
#816 = LINE ( 'NONE', #11223, #3260 ) ;
#817 = ORIENTED_EDGE ( 'NONE', *, *, #10768, .T. ) ;
#818 = CIRCLE ( 'NONE', #2648, 10.00000000000000000 ) ;
#819 = PLANE ( 'NONE',  #5906 ) ;
#820 = DIRECTION ( 'NONE',  ( -1.000000000000000000, 0.000000000000000000, 0.000000000000000000 ) ) ;
#821 = CARTESIAN_POINT ( 'NONE',  ( 24.27500000054622475, 13.07298590277314254, 93.04388485072563242 ) ) ;
#822 = DIRECTION ( 'NONE',  ( 0.000000000000000000, 0.000000000000000000, 1.000000000000000000 ) ) ;
#823 = CARTESIAN_POINT ( 'NONE',  ( 36.77500000054622831, 20.00000000000000355, 83.50966788445364841 ) ) ;
#824 = CARTESIAN_POINT ( 'NONE',  ( 29.67500000054622333, 24.28113015263587116, 96.68563167572563088 ) ) ;
#825 = CARTESIAN_POINT ( 'NONE',  ( 31.49999999999998224, 27.88596668178699645, 90.79316153445363113 ) ) ;
#826 = CIRCLE ( 'NONE', #8942, 0.5999999999999998668 ) ;
#827 = CARTESIAN_POINT ( 'NONE',  ( 30.79999999999998650, 15.59161060780646046, 84.72553407664153724 ) ) ;
#828 = CARTESIAN_POINT ( 'NONE',  ( 38.77500000054622831, 20.00000000000000355, 83.50966788445364841 ) ) ;
#829 = ORIENTED_EDGE ( 'NONE', *, *, #2173, .T. ) ;
#830 = CARTESIAN_POINT ( 'NONE',  ( 48.87500000054622262, 22.36655054427230382, 83.50966788445364841 ) ) ;
#831 = DIRECTION ( 'NONE',  ( -1.000000000000000000, 0.000000000000000000, 0.000000000000000000 ) ) ;
#832 = ORIENTED_EDGE ( 'NONE', *, *, #8899, .T. ) ;
#833 = EDGE_CURVE ( 'NONE', #4576, #10817, #6859, .T. ) ;
#834 =( REPRESENTATION_RELATIONSHIP ('NONE','NONE', #4262, #3370 ) REPRESENTATION_RELATIONSHIP_WITH_TRANSFORMATION ( #4942 )SHAPE_REPRESENTATION_RELATIONSHIP( ) );
#835 = CARTESIAN_POINT ( 'NONE',  ( -7.941295046835175953, 26.11247055527810446, -26.85294978034395186 ) ) ;
#836 = ORIENTED_EDGE ( 'NONE', *, *, #10882, .F. ) ;
#837 = CARTESIAN_POINT ( 'NONE',  ( 42.05000000109246372, 12.86707612778636012, 93.11078899226572503 ) ) ;
#838 = FACE_OUTER_BOUND ( 'NONE', #10049, .T. ) ;
#839 = CARTESIAN_POINT ( 'NONE',  ( 1.300460267930548142, 45.16099265032655552, -27.97162858364709592 ) ) ;
#840 = CARTESIAN_POINT ( 'NONE',  ( 42.07500000054622546, 15.71886984736413417, 96.68563167572563088 ) ) ;
#841 = FACE_OUTER_BOUND ( 'NONE', #8965, .T. ) ;
#842 = CARTESIAN_POINT ( 'NONE',  ( -0.6518953824324608126, 45.03170992320611532, -27.99428315319153526 ) ) ;
#843 = CARTESIAN_POINT ( 'NONE',  ( 44.67500000054621978, 15.71886984736413773, 84.90069139318163138 ) ) ;
#844 = CARTESIAN_POINT ( 'NONE',  ( 20.07500000054622546, 15.71886984736413417, 96.68563167572563088 ) ) ;
#845 = CARTESIAN_POINT ( 'NONE',  ( 6.000000000000000000, 2.919948986426526005, -5.057500000000003659 ) ) ;
#846 = DIRECTION ( 'NONE',  ( 0.000000000000000000, -1.039664082171044875E-15, -1.000000000000000000 ) ) ;
#847 = EDGE_LOOP ( 'NONE', ( #1862, #12124, #11567, #792 ) ) ;
#848 = CARTESIAN_POINT ( 'NONE',  ( 34.85000000109246798, 24.40838939219355197, 84.72553407664153724 ) ) ;
#849 = PRESENTATION_STYLE_ASSIGNMENT (( #5556 ) ) ;
#850 = VERTEX_POINT ( 'NONE', #2034 ) ;
#851 = CARTESIAN_POINT ( 'NONE',  ( 27.49999999999999645, 20.00000000000000355, 171.0000000000000000 ) ) ;
#852 = VERTEX_POINT ( 'NONE', #5027 ) ;
#853 = DIRECTION ( 'NONE',  ( -1.000000000000000000, -0.000000000000000000, -0.000000000000000000 ) ) ;
#854 = EDGE_CURVE ( 'NONE', #10832, #3939, #5915, .T. ) ;
#855 = CARTESIAN_POINT ( 'NONE',  ( 0.6627065662273624591, 10.01637405127483049, -20.99218728179891613 ) ) ;
#856 = CARTESIAN_POINT ( 'NONE',  ( 4.000000000000019540, 20.00000000000000711, 170.0000000000000000 ) ) ;
#857 = ADVANCED_FACE ( 'NONE', ( #1095 ), #4961, .F. ) ;
#858 = DIRECTION ( 'NONE',  ( 0.000000000000000000, 0.000000000000000000, 1.000000000000000000 ) ) ;
#859 = CARTESIAN_POINT ( 'NONE',  ( -3.305497356469124792, 46.23421970496524125, 20.73954946919153031 ) ) ;
#860 = ORIENTED_EDGE ( 'NONE', *, *, #4043, .T. ) ;
#861 = DIRECTION ( 'NONE',  ( 1.000000000000000000, 0.000000000000000000, 0.000000000000000000 ) ) ;
#862 = CARTESIAN_POINT ( 'NONE',  ( 48.05000000109247082, 12.86707612778636012, 93.11078899226572503 ) ) ;
#863 = CARTESIAN_POINT ( 'NONE',  ( 49.77500000054621410, 22.36655054427230027, 98.07665518445361386 ) ) ;
#864 = ORIENTED_EDGE ( 'NONE', *, *, #2205, .T. ) ;
#865 = LINE ( 'NONE', #4866, #9443 ) ;
#866 = CARTESIAN_POINT ( 'NONE',  ( 5.000000000000000888, 50.00000000000000000, -20.39607805437114152 ) ) ;
#867 = ORIENTED_EDGE ( 'NONE', *, *, #4196, .T. ) ;
#868 = EDGE_CURVE ( 'NONE', #10579, #6723, #10784, .T. ) ;
#869 = EDGE_LOOP ( 'NONE', ( #5985, #11323, #8486, #2065, #3594 ) ) ;
#870 = AXIS2_PLACEMENT_3D ( 'NONE', #1149, #3864, #4051 ) ;
#871 = CARTESIAN_POINT ( 'NONE',  ( 1.000000000000000888, 20.00000000000000355, 170.9999999999999716 ) ) ;
#872 = CARTESIAN_POINT ( 'NONE',  ( 0.000000000000000000, 0.000000000000000000, 0.000000000000000000 ) ) ;
#873 = EDGE_CURVE ( 'NONE', #2882, #5573, #4490, .T. ) ;
#874 = DIRECTION ( 'NONE',  ( -0.000000000000000000, 0.8660254037844395958, 0.4999999999999983902 ) ) ;
#875 = CARTESIAN_POINT ( 'NONE',  ( 10.00000000000000178, 0.000000000000000000, 0.000000000000000000 ) ) ;
#876 = AXIS2_PLACEMENT_3D ( 'NONE', #7275, #9190, #4239 ) ;
#877 = CARTESIAN_POINT ( 'NONE',  ( -3.051621101708449579, 53.97419359098365987, -20.77889715443343377 ) ) ;
#879 = EDGE_CURVE ( 'NONE', #7138, #8662, #3257, .T. ) ;
#878 = CARTESIAN_POINT ( 'NONE',  ( 3.061616997868383043E-15, 139.9999999999999716, 25.00000000000000000 ) ) ;
#880 = CARTESIAN_POINT ( 'NONE',  ( -21.00000000000001066, 77.00000000000000000, 154.3533255156881978 ) ) ;
#881 = DIRECTION ( 'NONE',  ( 1.000000000000000000, 0.000000000000000000, 0.000000000000000000 ) ) ;
#882 = ORIENTED_EDGE ( 'NONE', *, *, #9800, .T. ) ;
#883 = CARTESIAN_POINT ( 'NONE',  ( 19.71250000081934672, 20.00000000000000355, 98.18490835945361539 ) ) ;
#884 = CARTESIAN_POINT ( 'NONE',  ( -177.0000000000000000, 56.99999999999997868, 174.3533255156882262 ) ) ;
#885 = AXIS2_PLACEMENT_3D ( 'NONE', #7770, #5047, #2950 ) ;
#886 = VECTOR ( 'NONE', #11565, 1000.000000000000000 ) ;
#887 = CARTESIAN_POINT ( 'NONE',  ( 26.77500000054622120, 17.63344945572770328, 83.50966788445364841 ) ) ;
#888 = PRODUCT_DEFINITION_FORMATION_WITH_SPECIFIED_SOURCE ( 'ANY', '', #2946, .NOT_KNOWN. ) ;
#889 = CARTESIAN_POINT ( 'NONE',  ( 42.17500000054622689, 13.07298590277314254, 93.04388485072563242 ) ) ;
#890 = CARTESIAN_POINT ( 'NONE',  ( 24.77500000054622475, 17.63344945572770328, 83.50966788445364841 ) ) ;
#891 = CARTESIAN_POINT ( 'NONE',  ( 32.09999999999998721, 17.56310227825320425, 98.29316153445363113 ) ) ;
#892 = B_SPLINE_CURVE_WITH_KNOTS ( 'NONE', 3,
 ( #7213, #5385, #9191, #2454, #500, #2580, #12107, #6328, #621, #5570, #3473, #6450, #6268, #8421, #9439, #12291, #6510, #11087, #1687, #10141, #10312, #741, #4609, #5321, #1631, #4364, #9318, #8299 ),
 .UNSPECIFIED., .F., .F.,
 ( 4, 2, 2, 2, 2, 2, 2, 2, 2, 2, 2, 2, 2, 4 ),
 ( 0.04738593773884331589, 0.04935840384251231894, 0.05034463689434681699, 0.05133086994618132198, 0.05231710299801582004, 0.05330333604985031809, 0.05527580215351931420, 0.05626203520535381225, 0.05724826825718831030, 0.05922073436085731335, 0.06020696741269181834, 0.06119320046452632333, 0.06217943351636082833, 0.06316566656819533332 ),
 .UNSPECIFIED. ) ;
#893 = CARTESIAN_POINT ( 'NONE',  ( 34.69999999999998863, 13.62011893735970958, 86.15790661882942914 ) ) ;
#894 = CARTESIAN_POINT ( 'NONE',  ( 34.07500000054622546, 13.80429023900056507, 95.29460816699764791 ) ) ;
#895 = ORIENTED_EDGE ( 'NONE', *, *, #10610, .T. ) ;
#896 = CARTESIAN_POINT ( 'NONE',  ( 42.37500000054622262, 13.07298590277314432, 88.54243821818161564 ) ) ;
#897 = CARTESIAN_POINT ( 'NONE',  ( 28.05000000109246372, 12.86707612778636012, 93.11078899226572503 ) ) ;
#898 = ORIENTED_EDGE ( 'NONE', *, *, #12369, .F. ) ;
#899 = VECTOR ( 'NONE', #7447, 1000.000000000000114 ) ;
#900 = CARTESIAN_POINT ( 'NONE',  ( -2.283355574799413201, 29.74132092790486581, -27.90859578342948666 ) ) ;
#901 = EDGE_LOOP ( 'NONE', ( #6804, #8146, #864, #518, #4487 ) ) ;
#902 = CARTESIAN_POINT ( 'NONE',  ( 3.238656815135313671, 29.46670881375417395, -24.79134413122120151 ) ) ;
#903 = CARTESIAN_POINT ( 'NONE',  ( 32.69999999999999574, 13.62011893735970958, 86.15790661882942914 ) ) ;
#904 = CARTESIAN_POINT ( 'NONE',  ( 5.000000000000000000, 0.000000000000000000, 0.000000000000000000 ) ) ;
#905 = EDGE_CURVE ( 'NONE', #2831, #5337, #9640, .T. ) ;
#906 = CARTESIAN_POINT ( 'NONE',  ( 46.47500000054622404, 13.07298590277314432, 88.54243821818161564 ) ) ;
#907 = CARTESIAN_POINT ( 'NONE',  ( 91.03600000000000136, 0.000000000000000000, 0.000000000000000000 ) ) ;
#908 = EDGE_CURVE ( 'NONE', #10212, #10832, #6331, .T. ) ;
#909 =( LENGTH_UNIT ( ) NAMED_UNIT ( * ) SI_UNIT ( .MILLI., .METRE. ) );
#910 = CARTESIAN_POINT ( 'NONE',  ( 46.47500000054622404, 13.07298590277314432, 88.54243821818161564 ) ) ;
#911 = CARTESIAN_POINT ( 'NONE',  ( 46.79999999999999005, 15.59161060780646046, 84.72553407664153724 ) ) ;
#912 = AXIS2_PLACEMENT_3D ( 'NONE', #4671, #10433, #1744 ) ;
#913 = CARTESIAN_POINT ( 'NONE',  ( 41.99999999999998579, 20.00000000000000355, 98.29316153445363113 ) ) ;
#914 = CARTESIAN_POINT ( 'NONE',  ( 49.67500000054621978, 22.36655054427230027, 98.07665518445361386 ) ) ;
#915 = ORIENTED_EDGE ( 'NONE', *, *, #1713, .F. ) ;
#916 = CARTESIAN_POINT ( 'NONE',  ( 38.25000000109246656, 12.86707612778636012, 88.47553407664152303 ) ) ;
#917 = CARTESIAN_POINT ( 'NONE',  ( 8.667518415056527203, 14.97026592263945410, 23.45254893740142066 ) ) ;
#918 = VERTEX_POINT ( 'NONE', #1888 ) ;
#919 = EDGE_CURVE ( 'NONE', #6911, #10286, #8230, .T. ) ;
#920 = CARTESIAN_POINT ( 'NONE',  ( 12.59999999999999964, 0.000000000000000000, 0.000000000000000000 ) ) ;
#921 = ORIENTED_EDGE ( 'NONE', *, *, #7265, .F. ) ;
#922 = CARTESIAN_POINT ( 'NONE',  ( -2.290944097510326571, 29.73958545346254922, -24.89690719708686828 ) ) ;
#923=STYLED_ITEM('',(#12584),#10571);
#924 = CARTESIAN_POINT ( 'NONE',  ( 0.3308316500937774629, 9.999999999999994671, -21.00000000000000711 ) ) ;
#925 = CARTESIAN_POINT ( 'NONE',  ( -4.149932937002940747, 29.10413268181202184, 24.65505180927770112 ) ) ;
#926 = CARTESIAN_POINT ( 'NONE',  ( 37.87500000054622262, 17.63344945572769973, 98.07665518445361386 ) ) ;
#927 = FACE_OUTER_BOUND ( 'NONE', #11549, .T. ) ;
#928 = LINE ( 'NONE', #8541, #7268 ) ;
#929 = ORIENTED_EDGE ( 'NONE', *, *, #9179, .F. ) ;
#930 = EDGE_CURVE ( 'NONE', #5431, #4145, #2846, .T. ) ;
#931 = LINE ( 'NONE', #802, #8606 ) ;
#932 = LINE ( 'NONE', #8664, #7977 ) ;
#933 = CARTESIAN_POINT ( 'NONE',  ( 21.17500000054623044, 26.92701409722686634, 88.54243821818162985 ) ) ;
#934 = EDGE_LOOP ( 'NONE', ( #7388, #10470, #4956, #11399 ) ) ;
#935 = CARTESIAN_POINT ( 'NONE',  ( -31.89339828220177964, 27.49999999999999645, 140.6066017177982133 ) ) ;
#936 = DIRECTION ( 'NONE',  ( -1.000000000000000000, -0.000000000000000000, -0.000000000000000000 ) ) ;
#937 = ORIENTED_EDGE ( 'NONE', *, *, #4287, .F. ) ;
#938 = VERTEX_POINT ( 'NONE', #4530 ) ;
#939 = EDGE_CURVE ( 'NONE', #7259, #10526, #4687, .T. ) ;
#940 = VECTOR ( 'NONE', #3877, 1000.000000000000000 ) ;
#941 = CARTESIAN_POINT ( 'NONE',  ( -4.473766101552917540, 28.96742557902637927, -20.52713491992151162 ) ) ;
#942 = CARTESIAN_POINT ( 'NONE',  ( 41.35889894354065177, 20.00000000000000355, 162.0000000000000000 ) ) ;
#943 = CARTESIAN_POINT ( 'NONE',  ( 20.99999999999998579, 20.00000000000000355, 83.29316153445364534 ) ) ;
#944 = CARTESIAN_POINT ( 'NONE',  ( 11.99999999999999822, 0.000000000000000000, 0.000000000000000000 ) ) ;
#945 = CARTESIAN_POINT ( 'NONE',  ( 6.000000000000000000, 2.919948986426526005, -5.057500000000003659 ) ) ;
#946 = DIRECTION ( 'NONE',  ( -0.000000000000000000, -1.000000000000000000, -0.000000000000000000 ) ) ;
#947 = AXIS2_PLACEMENT_3D ( 'NONE', #5391, #1577, #1335 ) ;
#948 = CARTESIAN_POINT ( 'NONE',  ( 2.286402882168606432, 10.25929110584701931, 24.89734643733720176 ) ) ;
#949 = VERTEX_POINT ( 'NONE', #12428 ) ;
#950 = CARTESIAN_POINT ( 'NONE',  ( 1.326742001580319741, 29.91711497655587948, -24.96694321103489855 ) ) ;
#951 = UNCERTAINTY_MEASURE_WITH_UNIT (LENGTH_MEASURE( 1.000000000000000082E-05 ), #4583, 'distance_accuracy_value', 'NONE');
#952 = EDGE_CURVE ( 'NONE', #3847, #6680, #3726, .T. ) ;
#953 = PRODUCT_CONTEXT ( 'NONE', #7801, 'mechanical' ) ;
#954 = AXIS2_PLACEMENT_3D ( 'NONE', #4744, #1752, #9509 ) ;
#955 = CARTESIAN_POINT ( 'NONE',  ( 24.97500000054622049, 22.36655054427230382, 83.50966788445364841 ) ) ;
#956 = CARTESIAN_POINT ( 'NONE',  ( 47.67500000054622689, 24.28113015263587116, 96.68563167572563088 ) ) ;
#957 = CARTESIAN_POINT ( 'NONE',  ( 41.97500000054623115, 15.71886984736413417, 96.68563167572563088 ) ) ;
#958 = EDGE_CURVE ( 'NONE', #8162, #11970, #11300, .T. ) ;
#959 = CARTESIAN_POINT ( 'NONE',  ( 29.77500000054622120, 22.36655054427230027, 98.07665518445361386 ) ) ;
#960 = CARTESIAN_POINT ( 'NONE',  ( 27.59999999999999076, 27.13292387221364876, 93.11078899226573924 ) ) ;
#961 = CARTESIAN_POINT ( 'NONE',  ( 34.49999999999998579, 12.11403331821300533, 90.79316153445363113 ) ) ;
#962 = CARTESIAN_POINT ( 'NONE',  ( 31.97500000054623470, 15.71886984736413417, 96.68563167572563088 ) ) ;
#963 = ORIENTED_EDGE ( 'NONE', *, *, #640, .T. ) ;
#964 = LINE ( 'NONE', #12503, #10330 ) ;
#965 = VECTOR ( 'NONE', #5995, 1000.000000000000000 ) ;
#966 = ORIENTED_EDGE ( 'NONE', *, *, #49, .F. ) ;
#967 = CARTESIAN_POINT ( 'NONE',  ( 2.215581936987904843, 54.49413548860790257, 27.91383394955003183 ) ) ;
#968 = ORIENTED_EDGE ( 'NONE', *, *, #9389, .T. ) ;
#969 = CARTESIAN_POINT ( 'NONE',  ( 43.79999999999999005, 24.40838939219354842, 96.86078899226572503 ) ) ;
#970 = FACE_OUTER_BOUND ( 'NONE', #11386, .T. ) ;
#971 = ADVANCED_BREP_SHAPE_REPRESENTATION ( '', ( #6265, #9021 ), #4332 ) ;
#972 = CARTESIAN_POINT ( 'NONE',  ( 47.47500000054622404, 26.92701409722686634, 93.04388485072563242 ) ) ;
#973 = DIRECTION ( 'NONE',  ( 0.000000000000000000, 0.000000000000000000, -1.000000000000000000 ) ) ;
#974 = AXIS2_PLACEMENT_3D ( 'NONE', #12267, #776, #3567 ) ;
#975 = FACE_OUTER_BOUND ( 'NONE', #8889, .T. ) ;
#976 = CARTESIAN_POINT ( 'NONE',  ( 43.77500000054622120, 22.36655054427230027, 98.07665518445361386 ) ) ;
#977 = CARTESIAN_POINT ( 'NONE',  ( 21.37500000054622262, 27.65831843345427998, 90.79316153445363113 ) ) ;
#978 = CARTESIAN_POINT ( 'NONE',  ( -6.849710128414980836, 27.29284600759404356, -24.04449974210336904 ) ) ;
#979 = CARTESIAN_POINT ( 'NONE',  ( 6.000000000000000000, 8.759846959279592227, -5.057500000000009877 ) ) ;
#980 = ORIENTED_EDGE ( 'NONE', *, *, #75, .T. ) ;
#981 = CARTESIAN_POINT ( 'NONE',  ( 28.95000000109246585, 26.37988106264029398, 86.15790661882942914 ) ) ;
#982 = CARTESIAN_POINT ( 'NONE',  ( 6.110979747148361341, 12.05740682582580625, 24.24803741642852373 ) ) ;
#983 = ORIENTED_EDGE ( 'NONE', *, *, #3645, .F. ) ;
#984 = EDGE_LOOP ( 'NONE', ( #6494, #547, #3522, #403 ) ) ;
#985 = EDGE_CURVE ( 'NONE', #8822, #6118, #9067, .T. ) ;
#986 = DIRECTION ( 'NONE',  ( 1.000000000000000000, 0.000000000000000000, 0.000000000000000000 ) ) ;
#987 = FACE_OUTER_BOUND ( 'NONE', #9258, .T. ) ;
#988 = CARTESIAN_POINT ( 'NONE',  ( -31.74999999999995737, 9.797174393178825657E-16, -8.000000000000000000 ) ) ;
#989 = AXIS2_PLACEMENT_3D ( 'NONE', #9387, #11468, #6581 ) ;
#990 = CARTESIAN_POINT ( 'NONE',  ( 39.07500000054621836, 26.19570976099943493, 86.29171490190961435 ) ) ;
#991 = CARTESIAN_POINT ( 'NONE',  ( 35.77500000054622831, 22.36655054427230027, 98.07665518445361386 ) ) ;
#992 = CARTESIAN_POINT ( 'NONE',  ( -2.645127067179048996, 54.24614625768938225, 27.87511004317194718 ) ) ;
#993 = CARTESIAN_POINT ( 'NONE',  ( 7.945602540532026303, 26.10722575314713723, -26.85169520992049996 ) ) ;
#994 = CARTESIAN_POINT ( 'NONE',  ( 34.99999999999998579, 20.00000000000000000, 137.5000000000000000 ) ) ;
#995 = AXIS2_PLACEMENT_3D ( 'NONE', #11324, #486, #3395 ) ;
#996 = ORIENTED_EDGE ( 'NONE', *, *, #8532, .T. ) ;
#997 = LINE ( 'NONE', #6568, #10826 ) ;
#998 = DIRECTION ( 'NONE',  ( -0.000000000000000000, -0.000000000000000000, -1.000000000000000000 ) ) ;
#999 = ORIENTED_EDGE ( 'NONE', *, *, #11054, .F. ) ;
#1000 = DIRECTION ( 'NONE',  ( 0.000000000000000000, 0.000000000000000000, 1.000000000000000000 ) ) ;
#1001 = UNCERTAINTY_MEASURE_WITH_UNIT (LENGTH_MEASURE( 1.000000000000000082E-05 ), #909, 'distance_accuracy_value', 'NONE');
#1002 = CARTESIAN_POINT ( 'NONE',  ( 3.975237584097107923, 53.05037957731131826, -20.62115343197593020 ) ) ;
#1003 = ORIENTED_EDGE ( 'NONE', *, *, #6685, .F. ) ;
#1004 = ADVANCED_FACE ( 'NONE', ( #4240 ), #311, .F. ) ;
#1005=STYLED_ITEM('',(#12584),#6058);
#1006 = CARTESIAN_POINT ( 'NONE',  ( 6.000000000000000000, -2.919948986426523341, 5.057500000000002771 ) ) ;
#1007 = CIRCLE ( 'NONE', #1208, 7.500000000000000000 ) ;
#1008 = AXIS2_PLACEMENT_3D ( 'NONE', #4470, #7262, #4286 ) ;
#1009 = CARTESIAN_POINT ( 'NONE',  ( 43.55000000109247082, 22.43689772174677088, 98.29316153445365956 ) ) ;
#1010 = EDGE_CURVE ( 'NONE', #10421, #5573, #6897, .T. ) ;
#1011 = CARTESIAN_POINT ( 'NONE',  ( -50.00000000000001421, 22.00000000000000000, 152.2284161474004520 ) ) ;
#1012 = DIRECTION ( 'NONE',  ( -0.000000000000000000, -1.000000000000000000, -0.000000000000000000 ) ) ;
#1013 = FACE_OUTER_BOUND ( 'NONE', #6745, .T. ) ;
#1014 = DIRECTION ( 'NONE',  ( -0.000000000000000000, -1.000000000000000000, -0.000000000000000000 ) ) ;
#1015 = DIRECTION ( 'NONE',  ( 0.000000000000000000, -0.4999999999999990008, 0.8660254037844391517 ) ) ;
#1016 = CARTESIAN_POINT ( 'NONE',  ( 10.00000000000000178, 20.33006360438132987, -18.46618531261938756 ) ) ;
#1017 = VECTOR ( 'NONE', #8718, 1000.000000000000000 ) ;
#1018 = CARTESIAN_POINT ( 'NONE',  ( 8.975091145622032585, 15.54177410167867990, 23.33498156074052687 ) ) ;
#1019 = ORIENTED_EDGE ( 'NONE', *, *, #7656, .F. ) ;
#1020 = CARTESIAN_POINT ( 'NONE',  ( 6.844556472468130259, 27.29775667647069071, -24.04598060202682319 ) ) ;
#1021 = SHAPE_DEFINITION_REPRESENTATION ( #9949, #1739 ) ;
#1022 = AXIS2_PLACEMENT_3D ( 'NONE', #1034, #7809, #4955 ) ;
#1023 = ADVANCED_FACE ( 'NONE', ( #184 ), #3153, .T. ) ;
#1024 = CARTESIAN_POINT ( 'NONE',  ( 20.57500000054622191, 13.80429023900056684, 86.29171490190961435 ) ) ;
#1025 = CARTESIAN_POINT ( 'NONE',  ( 49.37500000054622973, 27.65831843345427998, 90.79316153445363113 ) ) ;
#1026 = CARTESIAN_POINT ( 'NONE',  ( 37.37500000054622973, 26.92701409722686634, 93.04388485072563242 ) ) ;
#1027 = CARTESIAN_POINT ( 'NONE',  ( 27.77500000054622475, 22.36655054427230027, 98.07665518445361386 ) ) ;
#1028 = CARTESIAN_POINT ( 'NONE',  ( 26.49999999999998934, 12.11403331821300533, 90.79316153445363113 ) ) ;
#1029 = EDGE_CURVE ( 'NONE', #667, #12368, #11254, .T. ) ;
#1030 = CARTESIAN_POINT ( 'NONE',  ( 32.87500000054622973, 22.36655054427230382, 83.50966788445364841 ) ) ;
#1031 = ORIENTED_EDGE ( 'NONE', *, *, #873, .F. ) ;
#1032 = COLOUR_RGB ( '',0.7921568627450980005, 0.8196078431372548767, 0.9333333333333333481 ) ;
#1033 = PRODUCT_DEFINITION_SHAPE ( 'NONE', 'NONE',  #12550 ) ;
#1034 = CARTESIAN_POINT ( 'NONE',  ( -5.000000000000000888, -3.000000000000002665, 218.7511230907454944 ) ) ;
#1035 = VERTEX_POINT ( 'NONE', #3161 ) ;
#1036 = DIRECTION ( 'NONE',  ( 0.000000000000000000, 0.000000000000000000, 1.000000000000000000 ) ) ;
#1037 = ORIENTED_EDGE ( 'NONE', *, *, #3690, .T. ) ;
#1038 = EDGE_CURVE ( 'NONE', #7452, #11818, #12078, .T. ) ;
#1039 = CARTESIAN_POINT ( 'NONE',  ( -2.000000000000015543, 20.00000000000000355, 83.29316153445364534 ) ) ;
#1040 = FACE_OUTER_BOUND ( 'NONE', #4242, .T. ) ;
#1041 = VECTOR ( 'NONE', #11538, 1000.000000000000000 ) ;
#1042 = CARTESIAN_POINT ( 'NONE',  ( 46.17500000054622689, 13.80429023900056507, 95.29460816699764791 ) ) ;
#1043 = FACE_OUTER_BOUND ( 'NONE', #6289, .T. ) ;
#1044 = DIRECTION ( 'NONE',  ( -0.000000000000000000, -1.000000000000000000, -0.000000000000000000 ) ) ;
#1045 = CARTESIAN_POINT ( 'NONE',  ( 46.87500000054622262, 20.00000000000000355, 83.50966788445364841 ) ) ;
#1046 = CARTESIAN_POINT ( 'NONE',  ( 43.09999999999998721, 22.43689772174679575, 83.29316153445363113 ) ) ;
#1047 = CARTESIAN_POINT ( 'NONE',  ( 39.99999999999998579, 20.00000000000000355, 98.29316153445363113 ) ) ;
#1048 = CARTESIAN_POINT ( 'NONE',  ( 43.99999999999999289, 20.00000000000000355, 98.29316153445363113 ) ) ;
#1049 = ORIENTED_EDGE ( 'NONE', *, *, #3891, .T. ) ;
#1050 = CARTESIAN_POINT ( 'NONE',  ( 29.95000000109246585, 13.62011893735971135, 95.42841645007781892 ) ) ;
#1051 = CARTESIAN_POINT ( 'NONE',  ( -4.466051270639568749, 11.02833005318139925, 24.60558887372674519 ) ) ;
#1052 = ORIENTED_EDGE ( 'NONE', *, *, #3804, .T. ) ;
#1053 = ORIENTED_EDGE ( 'NONE', *, *, #1765, .F. ) ;
#1054 = LINE ( 'NONE', #12403, #3624 ) ;
#1055 = DIRECTION ( 'NONE',  ( -1.000000000000000000, 0.000000000000000000, 0.000000000000000000 ) ) ;
#1056 = FACE_OUTER_BOUND ( 'NONE', #10210, .T. ) ;
#1057 = CARTESIAN_POINT ( 'NONE',  ( 39.47500000054623115, 26.19570976099943493, 95.29460816699764791 ) ) ;
#1058 = CARTESIAN_POINT ( 'NONE',  ( 31.37500000054622618, 27.65831843345427998, 90.79316153445363113 ) ) ;
#1059 = CARTESIAN_POINT ( 'NONE',  ( -9.983660626454435416, 20.66196728388187864, 18.47506278258854806 ) ) ;
#1060 = CARTESIAN_POINT ( 'NONE',  ( 33.79382810696422013, 25.37779564132841159, 151.2938281069642130 ) ) ;
#1061 = ORIENTED_EDGE ( 'NONE', *, *, #10505, .T. ) ;
#1062 = DIRECTION ( 'NONE',  ( -0.000000000000000000, -1.000000000000000000, -0.000000000000000000 ) ) ;
#1063 = ORIENTED_EDGE ( 'NONE', *, *, #1474, .F. ) ;
#1064 = CARTESIAN_POINT ( 'NONE',  ( -50.00000000000001421, 22.00000000000000000, 169.9999999999999716 ) ) ;
#1065 = ORIENTED_EDGE ( 'NONE', *, *, #2468, .F. ) ;
#1066 = EDGE_LOOP ( 'NONE', ( #393, #7519, #11014, #6682 ) ) ;
#1067 = FACE_OUTER_BOUND ( 'NONE', #12430, .T. ) ;
#1068 = CARTESIAN_POINT ( 'NONE',  ( 2.504881716134078395, 54.33965200799452333, 24.87570091612971979 ) ) ;
#1069 = CARTESIAN_POINT ( 'NONE',  ( 7.054895033614133837, 27.09199502823383909, 88.30591582403000928 ) ) ;
#1070 = EDGE_CURVE ( 'NONE', #10817, #1347, #4044, .T. ) ;
#1071 = CARTESIAN_POINT ( 'NONE',  ( -5.000000000000000000, 50.00000000000000000, -24.49489742783178059 ) ) ;
#1072 = CARTESIAN_POINT ( 'NONE',  ( 4.490871182873028111, 47.77729020916527958, -20.51460075614775036 ) ) ;
#1073 =( BOUNDED_SURFACE ( )  B_SPLINE_SURFACE ( 1, 2, ( 
 ( #236, #3902, #1190, #5055, #11837, #9940, #1248, #7780, #6822, #7905, #1997, #11711, #4093, #7014, #2197, #5119, #8984, #10748, #9750, #8851, #5939, #4159, #4029, #11774, #3079, #7197, #7135, #1313, #542, #8160, #1492, #2264, #11073, #7260, #1559, #9301, #11009, #361, #8346, #10128, #5369, #4405, #9114, #2440, #5242, #4467, #3392, #421, #2323, #12027, #11134, #3331, #6317, #3514, #2503, #10185, #6131, #5182, #5429, #2379, #6377, #4283, #1375, #6189, #6250, #5307, #8222, #11964, #10244, #10064, #1438, #3274, #9175, #9050, #606, #12212, #8283, #483, #7323, #4349, #3459, #12090, #9239, #7386, #12152, #4227, #10002, #8099, #3760, #5495, #12397, #11505, #3697, #6614, #7577, #2562, #1735, #9364, #4595, #2814, #5740, #1616, #6678, #8588, #3635, #665, #10547, #9550, #9487, #9608, #4531, #2691, #11383, #5614, #916, #12458, #12337, #787, #8466, #6434, #2754, #7513, #8406, #4784, #8649, #11321, #7640, #6495, #11255, #8525, #5555, #4656, #6555, #10298, #12521, #3826, #1858, #1795, #12278, #3575, #7450, #2628, #10359, #1673, #11444, #9425, #10484, #726, #848, #10422, #5680, #4717, #10671, #6928, #11569, #10604, #11758, #1980, #7763, #4911, #155, #8772, #4012, #8966, #7954, #3066, #7701, #6741, #6995, #3954, #4076, #9734, #6805, #11636, #7828, #10733, #1108, #4847, #11820, #25, #91, #8713, #5864, #1917, #3128, #2178, #9861, #3888, #220, #6870, #8902, #11696, #4974, #9923, #7889, #5800, #1232, #1050, #10866, #9672, #8836, #6050, #10797, #2110, #5987, #2877, #2045, #981, #3002, #5101, #280, #2940, #5925, #5037, #9797, #1175, #3443, #2423, #2365, #2483, #9984, #8144, #4268, #11058, #11180, #5350, #5227, #7181, #1360, #11888, #8206, #9097, #1294, #6360, #10227, #4209, #1477, #11950, #4143, #1421, #10995, #6236, #405, #8017, #1540, #5413, #528, #7245, #5167, #9222, #3194, #4388, #8266, #9034, #9160, #7055, #465, #9284, #6300, #10933, #12135, #2247, #7121, #3375, #6114, #346, #12074, #10050, #11117, #8082, #12010, #4328, #7307, #3254, #2305, #6174, #3314, #10110, #10170, #5289, #7433, #768, #3560, #2796, #1718, #10282, #12383, #9347, #11304, #10405, #3617, #4578, #4513, #3742, #4637, #4700, #1659, #6418, #11428, #9407, #8572 ),
 ( #2610, #7497, #10342, #11486, #8449, #5540, #1599, #8508, #6479, #830, #12318, #10528, #3681, #9532, #6596, #5598, #650, #7369, #12443, #710, #10464, #5480, #8389, #11367, #2674, #6537, #9470, #12258, #7559, #2739, #1775, #5659, #7623, #6659, #3497, #1840, #5722, #587, #4453, #8331, #12197, #11238, #2546, #4177, #313, #8632, #7859, #5072, #10020, #1141, #11855, #251, #4107, #9001, #3162, #11788, #1329, #2143, #9589, #11919, #1263, #8938, #9829, #3093, #10763, #123, #9957, #6145, #6019, #7027, #5134, #7088, #8053, #3227, #896, #7987, #10969, #2277, #4767, #3982, #10901, #2216, #11730, #3033, #6086, #6898, #2074, #5954, #5005, #8870, #9892, #186, #4045, #7922, #6961, #10830, #10615, #9743, #3961, #12234, #10381, #1636, #7473, #1057, #2586, #9681, #8781, #990, #3896, #4856, #3537, #11579, #6458, #1866, #101, #3010, #11279, #7837, #5871, #926, #10319, #11706, #6816, #6750, #6878, #5516, #12529, #8659, #2887, #10742, #4919, #9619, #1927, #5748, #7410, #34, #4794, #9384, #2053, #5933, #8427, #9806, #3597, #8365, #5808, #2653, #8721, #3837, #686, #1117, #4553, #12297, #11644, #11347, #6516, #7711, #7773, #2951, #10679, #1990, #8844, #9993, #10122, #7129, #2375, #415, #6244, #7961, #4220, #164, #7897, #9045, #10878, #8092, #4983, #1241, #1306, #4276, #12020, #9870, #3073, #11068, #290, #11958, #11003, #11829, #5176, #3137, #7191, #6125, #7008, #5049, #2189, #356, #6060, #3267, #4022, #5236, #2315, #11767, #6936, #8154, #5112, #1370, #9933, #4086, #8910, #8976, #8028, #10943, #2120, #9108, #1183, #4153, #5997, #11899, #10804, #3324, #229, #6184, #3204, #10059, #7066, #2256, #11190, #7379, #3630, #6430, #4342, #7507, #12146, #10178, #4400, #11249, #4462, #5424, #5362, #4588, #5490, #5550, #2496, #7254, #12271, #10238, #9419, #8461, #1486, #2684, #12330, #9359, #11128, #6490, #476, #10353, #11315, #2434, #10292, #5300, #1610, #6549, #3569, #11379, #721, #1433, #8277, #659, #9169, #8216, #4524, #7318, #8400, #12085, #1551, #7445, #3387, #6312, #9233, #537, #3454, #9295, #2622, #1668, #6371, #600, #8341, #12207, #2556, #3508, #5315, #12099, #7330, #7269, #11201, #3584, #2571, #10250, #2330, #1382, #1622, #6323, #11265 ) ),
 .UNSPECIFIED., .F., .F., .F. ) 
 B_SPLINE_SURFACE_WITH_KNOTS ( ( 2, 2 ),
 ( 3, 2, 2, 2, 2, 2, 2, 2, 2, 2, 2, 2, 2, 2, 2, 2, 2, 2, 2, 2, 2, 2, 2, 2, 2, 2, 2, 2, 2, 2, 2, 2, 2, 2, 2, 2, 2, 2, 2, 2, 2, 2, 2, 2, 2, 2, 2, 2, 2, 2, 2, 2, 2, 2, 2, 2, 2, 2, 2, 2, 2, 2, 2, 2, 2, 2, 2, 2, 2, 2, 2, 2, 2, 2, 2, 2, 2, 2, 2, 2, 2, 2, 2, 2, 2, 2, 2, 2, 2, 2, 2, 2, 2, 2, 2, 2, 2, 2, 2, 2, 2, 2, 2, 2, 2, 2, 2, 2, 2, 2, 2, 2, 2, 2, 2, 2, 2, 2, 2, 2, 2, 2, 2, 2, 2, 2, 2, 2, 2, 2, 2, 2, 2, 2, 2, 2, 2, 2, 2, 2, 2, 2, 2, 2, 2, 2, 2, 2, 2, 2, 3 ),
 ( 0.000000000000000000, 1.000000000000000000 ),
 ( 0.000000000000000000, 0.006666666666666667095, 0.01333333333333333419, 0.02000000000000000042, 0.02666666666666666838, 0.03333333333333333287, 0.04000000000000000083, 0.04666666666666666879, 0.05333333333333333676, 0.05999999999999999778, 0.06666666666666666574, 0.07333333333333333370, 0.08000000000000000167, 0.08666666666666666963, 0.09333333333333333759, 0.1000000000000000056, 0.1066666666666666735, 0.1133333333333333276, 0.1199999999999999956, 0.1266666666666666774, 0.1333333333333333315, 0.1400000000000000133, 0.1466666666666666674, 0.1533333333333333215, 0.1600000000000000033, 0.1666666666666666574, 0.1733333333333333393, 0.1799999999999999933, 0.1866666666666666752, 0.1933333333333333293, 0.2000000000000000111, 0.2066666666666666652, 0.2133333333333333470, 0.2200000000000000011, 0.2266666666666666552, 0.2333333333333333370, 0.2399999999999999911, 0.2466666666666666730, 0.2533333333333333548, 0.2600000000000000089, 0.2666666666666666630, 0.2733333333333333171, 0.2800000000000000266, 0.2866666666666666807, 0.2933333333333333348, 0.2999999999999999889, 0.3066666666666666430, 0.3133333333333333526, 0.3200000000000000067, 0.3266666666666666607, 0.3333333333333333148, 0.3400000000000000244, 0.3466666666666666785, 0.3533333333333333326, 0.3599999999999999867, 0.3666666666666666408, 0.3733333333333333504, 0.3800000000000000044, 0.3866666666666666585, 0.3933333333333333126, 0.4000000000000000222, 0.4066666666666666763, 0.4133333333333333304, 0.4199999999999999845, 0.4266666666666666941, 0.4333333333333333481, 0.4400000000000000022, 0.4466666666666666563, 0.4533333333333333104, 0.4600000000000000200, 0.4666666666666666741, 0.4733333333333333282, 0.4799999999999999822, 0.4866666666666666918, 0.4933333333333333459, 0.5000000000000000000, 0.5066666666666667096, 0.5133333333333333082, 0.5200000000000000178, 0.5266666666666666163, 0.5333333333333333259, 0.5400000000000000355, 0.5466666666666666341, 0.5533333333333333437, 0.5600000000000000533, 0.5666666666666666519, 0.5733333333333333615, 0.5799999999999999600, 0.5866666666666666696, 0.5933333333333333792, 0.5999999999999999778, 0.6066666666666666874, 0.6133333333333332860, 0.6199999999999999956, 0.6266666666666667052, 0.6333333333333333037, 0.6400000000000000133, 0.6466666666666666119, 0.6533333333333333215, 0.6600000000000000311, 0.6666666666666666297, 0.6733333333333333393, 0.6800000000000000488, 0.6866666666666666474, 0.6933333333333333570, 0.6999999999999999556, 0.7066666666666666652, 0.7133333333333333748, 0.7199999999999999734, 0.7266666666666666829, 0.7333333333333332815, 0.7399999999999999911, 0.7466666666666667007, 0.7533333333333332993, 0.7600000000000000089, 0.7666666666666667185, 0.7733333333333333171, 0.7800000000000000266, 0.7866666666666666252, 0.7933333333333333348, 0.8000000000000000444, 0.8066666666666666430, 0.8133333333333333526, 0.8199999999999999512, 0.8266666666666666607, 0.8333333333333333703, 0.8399999999999999689, 0.8466666666666666785, 0.8533333333333333881, 0.8599999999999999867, 0.8666666666666666963, 0.8733333333333332948, 0.8800000000000000044, 0.8866666666666667140, 0.8933333333333333126, 0.9000000000000000222, 0.9066666666666666208, 0.9133333333333333304, 0.9200000000000000400, 0.9266666666666666385, 0.9333333333333333481, 0.9399999999999999467, 0.9466666666666666563, 0.9533333333333333659, 0.9599999999999999645, 0.9666666666666666741, 0.9733333333333333837, 0.9799999999999999822, 0.9866666666666666918, 0.9933333333333332904, 1.000000000000000000 ),
 .UNSPECIFIED. ) 
 GEOMETRIC_REPRESENTATION_ITEM ( )  RATIONAL_B_SPLINE_SURFACE ( (
 ( 1.000000000000000000, 0.9510565162951535312, 1.000000000000000000, 0.9510565162951535312, 1.000000000000000000, 0.9510565162951535312, 1.000000000000000000, 0.9510565162951535312, 1.000000000000000000, 0.9510565162951535312, 1.000000000000000000, 0.9510565162951535312, 1.000000000000000000, 0.9510565162951535312, 1.000000000000000000, 0.9510565162951535312, 1.000000000000000000, 0.9510565162951535312, 1.000000000000000000, 0.9510565162951535312, 1.000000000000000000, 0.9510565162951535312, 1.000000000000000000, 0.9510565162951535312, 1.000000000000000000, 0.9510565162951535312, 1.000000000000000000, 0.9510565162951535312, 1.000000000000000000, 0.9510565162951535312, 1.000000000000000000, 0.9510565162951535312, 1.000000000000000000, 0.9510565162951535312, 1.000000000000000000, 0.9510565162951535312, 1.000000000000000000, 0.9510565162951535312, 1.000000000000000000, 0.9510565162951535312, 1.000000000000000000, 0.9510565162951535312, 1.000000000000000000, 0.9510565162951535312, 1.000000000000000000, 0.9510565162951535312, 1.000000000000000000, 0.9510565162951535312, 1.000000000000000000, 0.9510565162951535312, 1.000000000000000000, 0.9510565162951535312, 1.000000000000000000, 0.9510565162951535312, 1.000000000000000000, 0.9510565162951535312, 1.000000000000000000, 0.9510565162951535312, 1.000000000000000000, 0.9510565162951535312, 1.000000000000000000, 0.9510565162951535312, 1.000000000000000000, 0.9510565162951535312, 1.000000000000000000, 0.9510565162951535312, 1.000000000000000000, 0.9510565162951535312, 1.000000000000000000, 0.9510565162951535312, 1.000000000000000000, 0.9510565162951535312, 1.000000000000000000, 0.9510565162951535312, 1.000000000000000000, 0.9510565162951535312, 1.000000000000000000, 0.9510565162951535312, 1.000000000000000000, 0.9510565162951535312, 1.000000000000000000, 0.9510565162951535312, 1.000000000000000000, 0.9510565162951535312, 1.000000000000000000, 0.9510565162951535312, 1.000000000000000000, 0.9510565162951535312, 1.000000000000000000, 0.9510565162951535312, 1.000000000000000000, 0.9510565162951535312, 1.000000000000000000, 0.9510565162951535312, 1.000000000000000000, 0.9510565162951535312, 1.000000000000000000, 0.9510565162951535312, 1.000000000000000000, 0.9510565162951535312, 1.000000000000000000, 0.9510565162951535312, 1.000000000000000000, 0.9510565162951535312, 1.000000000000000000, 0.9510565162951535312, 1.000000000000000000, 0.9510565162951535312, 1.000000000000000000, 0.9510565162951535312, 1.000000000000000000, 0.9510565162951535312, 1.000000000000000000, 0.9510565162951535312, 1.000000000000000000, 0.9510565162951535312, 1.000000000000000000, 0.9510565162951535312, 1.000000000000000000, 0.9510565162951535312, 1.000000000000000000, 0.9510565162951535312, 1.000000000000000000, 0.9510565162951535312, 1.000000000000000000, 0.9510565162951535312, 1.000000000000000000, 0.9510565162951535312, 1.000000000000000000, 0.9510565162951535312, 1.000000000000000000, 0.9510565162951535312, 1.000000000000000000, 0.9510565162951535312, 1.000000000000000000, 0.9510565162951535312, 1.000000000000000000, 0.9510565162951535312, 1.000000000000000000, 0.9510565162951535312, 1.000000000000000000, 0.9510565162951535312, 1.000000000000000000, 0.9510565162951535312, 1.000000000000000000, 0.9510565162951535312, 1.000000000000000000, 0.9510565162951535312, 1.000000000000000000, 0.9510565162951535312, 1.000000000000000000, 0.9510565162951535312, 1.000000000000000000, 0.9510565162951535312, 1.000000000000000000, 0.9510565162951535312, 1.000000000000000000, 0.9510565162951535312, 1.000000000000000000, 0.9510565162951535312, 1.000000000000000000, 0.9510565162951535312, 1.000000000000000000, 0.9510565162951535312, 1.000000000000000000, 0.9510565162951535312, 1.000000000000000000, 0.9510565162951535312, 1.000000000000000000, 0.9510565162951535312, 1.000000000000000000, 0.9510565162951535312, 1.000000000000000000, 0.9510565162951535312, 1.000000000000000000, 0.9510565162951535312, 1.000000000000000000, 0.9510565162951535312, 1.000000000000000000, 0.9510565162951535312, 1.000000000000000000, 0.9510565162951535312, 1.000000000000000000, 0.9510565162951535312, 1.000000000000000000, 0.9510565162951535312, 1.000000000000000000, 0.9510565162951535312, 1.000000000000000000, 0.9510565162951535312, 1.000000000000000000, 0.9510565162951535312, 1.000000000000000000, 0.9510565162951535312, 1.000000000000000000, 0.9510565162951535312, 1.000000000000000000, 0.9510565162951535312, 1.000000000000000000, 0.9510565162951535312, 1.000000000000000000, 0.9510565162951535312, 1.000000000000000000, 0.9510565162951535312, 1.000000000000000000, 0.9510565162951535312, 1.000000000000000000, 0.9510565162951535312, 1.000000000000000000, 0.9510565162951535312, 1.000000000000000000, 0.9510565162951535312, 1.000000000000000000, 0.9510565162951535312, 1.000000000000000000, 0.9510565162951535312, 1.000000000000000000, 0.9510565162951535312, 1.000000000000000000, 0.9510565162951535312, 1.000000000000000000, 0.9510565162951535312, 1.000000000000000000, 0.9510565162951535312, 1.000000000000000000, 0.9510565162951535312, 1.000000000000000000, 0.9510565162951535312, 1.000000000000000000, 0.9510565162951535312, 1.000000000000000000, 0.9510565162951535312, 1.000000000000000000, 0.9510565162951535312, 1.000000000000000000, 0.9510565162951535312, 1.000000000000000000, 0.9510565162951535312, 1.000000000000000000, 0.9510565162951535312, 1.000000000000000000, 0.9510565162951535312, 1.000000000000000000, 0.9510565162951535312, 1.000000000000000000, 0.9510565162951535312, 1.000000000000000000, 0.9510565162951535312, 1.000000000000000000, 0.9510565162951535312, 1.000000000000000000, 0.9510565162951535312, 1.000000000000000000, 0.9510565162951535312, 1.000000000000000000, 0.9510565162951535312, 1.000000000000000000, 0.9510565162951535312, 1.000000000000000000, 0.9510565162951535312, 1.000000000000000000, 0.9510565162951535312, 1.000000000000000000, 0.9510565162951535312, 1.000000000000000000, 0.9510565162951535312, 1.000000000000000000, 0.9510565162951535312, 1.000000000000000000, 0.9510565162951535312, 1.000000000000000000, 0.9510565162951535312, 1.000000000000000000, 0.9510565162951535312, 1.000000000000000000, 0.9510565162951535312, 1.000000000000000000, 0.9510565162951535312, 1.000000000000000000, 0.9510565162951535312, 1.000000000000000000, 0.9510565162951535312, 1.000000000000000000, 0.9510565162951535312, 1.000000000000000000, 0.9510565162951535312, 1.000000000000000000, 0.9510565162951535312, 1.000000000000000000, 0.9510565162951535312, 1.000000000000000000, 0.9510565162951535312, 1.000000000000000000, 0.9510565162951535312, 1.000000000000000000, 0.9510565162951535312, 1.000000000000000000, 0.9510565162951535312, 1.000000000000000000, 0.9510565162951535312, 1.000000000000000000),
 ( 1.000000000000000000, 0.9510565162951535312, 1.000000000000000000, 0.9510565162951535312, 1.000000000000000000, 0.9510565162951535312, 1.000000000000000000, 0.9510565162951535312, 1.000000000000000000, 0.9510565162951535312, 1.000000000000000000, 0.9510565162951535312, 1.000000000000000000, 0.9510565162951535312, 1.000000000000000000, 0.9510565162951535312, 1.000000000000000000, 0.9510565162951535312, 1.000000000000000000, 0.9510565162951535312, 1.000000000000000000, 0.9510565162951535312, 1.000000000000000000, 0.9510565162951535312, 1.000000000000000000, 0.9510565162951535312, 1.000000000000000000, 0.9510565162951535312, 1.000000000000000000, 0.9510565162951535312, 1.000000000000000000, 0.9510565162951535312, 1.000000000000000000, 0.9510565162951535312, 1.000000000000000000, 0.9510565162951535312, 1.000000000000000000, 0.9510565162951535312, 1.000000000000000000, 0.9510565162951535312, 1.000000000000000000, 0.9510565162951535312, 1.000000000000000000, 0.9510565162951535312, 1.000000000000000000, 0.9510565162951535312, 1.000000000000000000, 0.9510565162951535312, 1.000000000000000000, 0.9510565162951535312, 1.000000000000000000, 0.9510565162951535312, 1.000000000000000000, 0.9510565162951535312, 1.000000000000000000, 0.9510565162951535312, 1.000000000000000000, 0.9510565162951535312, 1.000000000000000000, 0.9510565162951535312, 1.000000000000000000, 0.9510565162951535312, 1.000000000000000000, 0.9510565162951535312, 1.000000000000000000, 0.9510565162951535312, 1.000000000000000000, 0.9510565162951535312, 1.000000000000000000, 0.9510565162951535312, 1.000000000000000000, 0.9510565162951535312, 1.000000000000000000, 0.9510565162951535312, 1.000000000000000000, 0.9510565162951535312, 1.000000000000000000, 0.9510565162951535312, 1.000000000000000000, 0.9510565162951535312, 1.000000000000000000, 0.9510565162951535312, 1.000000000000000000, 0.9510565162951535312, 1.000000000000000000, 0.9510565162951535312, 1.000000000000000000, 0.9510565162951535312, 1.000000000000000000, 0.9510565162951535312, 1.000000000000000000, 0.9510565162951535312, 1.000000000000000000, 0.9510565162951535312, 1.000000000000000000, 0.9510565162951535312, 1.000000000000000000, 0.9510565162951535312, 1.000000000000000000, 0.9510565162951535312, 1.000000000000000000, 0.9510565162951535312, 1.000000000000000000, 0.9510565162951535312, 1.000000000000000000, 0.9510565162951535312, 1.000000000000000000, 0.9510565162951535312, 1.000000000000000000, 0.9510565162951535312, 1.000000000000000000, 0.9510565162951535312, 1.000000000000000000, 0.9510565162951535312, 1.000000000000000000, 0.9510565162951535312, 1.000000000000000000, 0.9510565162951535312, 1.000000000000000000, 0.9510565162951535312, 1.000000000000000000, 0.9510565162951535312, 1.000000000000000000, 0.9510565162951535312, 1.000000000000000000, 0.9510565162951535312, 1.000000000000000000, 0.9510565162951535312, 1.000000000000000000, 0.9510565162951535312, 1.000000000000000000, 0.9510565162951535312, 1.000000000000000000, 0.9510565162951535312, 1.000000000000000000, 0.9510565162951535312, 1.000000000000000000, 0.9510565162951535312, 1.000000000000000000, 0.9510565162951535312, 1.000000000000000000, 0.9510565162951535312, 1.000000000000000000, 0.9510565162951535312, 1.000000000000000000, 0.9510565162951535312, 1.000000000000000000, 0.9510565162951535312, 1.000000000000000000, 0.9510565162951535312, 1.000000000000000000, 0.9510565162951535312, 1.000000000000000000, 0.9510565162951535312, 1.000000000000000000, 0.9510565162951535312, 1.000000000000000000, 0.9510565162951535312, 1.000000000000000000, 0.9510565162951535312, 1.000000000000000000, 0.9510565162951535312, 1.000000000000000000, 0.9510565162951535312, 1.000000000000000000, 0.9510565162951535312, 1.000000000000000000, 0.9510565162951535312, 1.000000000000000000, 0.9510565162951535312, 1.000000000000000000, 0.9510565162951535312, 1.000000000000000000, 0.9510565162951535312, 1.000000000000000000, 0.9510565162951535312, 1.000000000000000000, 0.9510565162951535312, 1.000000000000000000, 0.9510565162951535312, 1.000000000000000000, 0.9510565162951535312, 1.000000000000000000, 0.9510565162951535312, 1.000000000000000000, 0.9510565162951535312, 1.000000000000000000, 0.9510565162951535312, 1.000000000000000000, 0.9510565162951535312, 1.000000000000000000, 0.9510565162951535312, 1.000000000000000000, 0.9510565162951535312, 1.000000000000000000, 0.9510565162951535312, 1.000000000000000000, 0.9510565162951535312, 1.000000000000000000, 0.9510565162951535312, 1.000000000000000000, 0.9510565162951535312, 1.000000000000000000, 0.9510565162951535312, 1.000000000000000000, 0.9510565162951535312, 1.000000000000000000, 0.9510565162951535312, 1.000000000000000000, 0.9510565162951535312, 1.000000000000000000, 0.9510565162951535312, 1.000000000000000000, 0.9510565162951535312, 1.000000000000000000, 0.9510565162951535312, 1.000000000000000000, 0.9510565162951535312, 1.000000000000000000, 0.9510565162951535312, 1.000000000000000000, 0.9510565162951535312, 1.000000000000000000, 0.9510565162951535312, 1.000000000000000000, 0.9510565162951535312, 1.000000000000000000, 0.9510565162951535312, 1.000000000000000000, 0.9510565162951535312, 1.000000000000000000, 0.9510565162951535312, 1.000000000000000000, 0.9510565162951535312, 1.000000000000000000, 0.9510565162951535312, 1.000000000000000000, 0.9510565162951535312, 1.000000000000000000, 0.9510565162951535312, 1.000000000000000000, 0.9510565162951535312, 1.000000000000000000, 0.9510565162951535312, 1.000000000000000000, 0.9510565162951535312, 1.000000000000000000, 0.9510565162951535312, 1.000000000000000000, 0.9510565162951535312, 1.000000000000000000, 0.9510565162951535312, 1.000000000000000000, 0.9510565162951535312, 1.000000000000000000, 0.9510565162951535312, 1.000000000000000000, 0.9510565162951535312, 1.000000000000000000, 0.9510565162951535312, 1.000000000000000000, 0.9510565162951535312, 1.000000000000000000, 0.9510565162951535312, 1.000000000000000000, 0.9510565162951535312, 1.000000000000000000, 0.9510565162951535312, 1.000000000000000000, 0.9510565162951535312, 1.000000000000000000, 0.9510565162951535312, 1.000000000000000000, 0.9510565162951535312, 1.000000000000000000, 0.9510565162951535312, 1.000000000000000000, 0.9510565162951535312, 1.000000000000000000, 0.9510565162951535312, 1.000000000000000000, 0.9510565162951535312, 1.000000000000000000, 0.9510565162951535312, 1.000000000000000000, 0.9510565162951535312, 1.000000000000000000, 0.9510565162951535312, 1.000000000000000000, 0.9510565162951535312, 1.000000000000000000, 0.9510565162951535312, 1.000000000000000000, 0.9510565162951535312, 1.000000000000000000, 0.9510565162951535312, 1.000000000000000000, 0.9510565162951535312, 1.000000000000000000, 0.9510565162951535312, 1.000000000000000000) ) ) 
 REPRESENTATION_ITEM ( '' )  SURFACE ( )  );
#1074 = CARTESIAN_POINT ( 'NONE',  ( 4.838434350898961789, 48.69698515325892885, 27.57886596078574115 ) ) ;
#1075 = AXIS2_PLACEMENT_3D ( 'NONE', #9726, #10725, #10926 ) ;
#1076 = DIRECTION ( 'NONE',  ( 0.000000000000000000, 0.000000000000000000, -1.000000000000000000 ) ) ;
#1077 = ORIENTED_EDGE ( 'NONE', *, *, #11859, .T. ) ;
#1078 = CARTESIAN_POINT ( 'NONE',  ( -0.6564146843885075855, 10.01611589608920383, -27.99423190741217127 ) ) ;
#1079 = APPLICATION_PROTOCOL_DEFINITION ( 'draft international standard', 'automotive_design', 1998, #1328 ) ;
#1080 = CARTESIAN_POINT ( 'NONE',  ( 46.39999999999999147, 12.86707612778636012, 93.11078899226572503 ) ) ;
#1081 = CARTESIAN_POINT ( 'NONE',  ( 23.95000000109246585, 13.62011893735970958, 95.42841645007781892 ) ) ;
#1082 = CIRCLE ( 'NONE', #11409, 17.49999999999996803 ) ;
#1083 = CARTESIAN_POINT ( 'NONE',  ( 31.47500000054623115, 26.19570976099943849, 95.29460816699764791 ) ) ;
#1084 = CARTESIAN_POINT ( 'NONE',  ( 1.648701702613829090, 10.13131270077370338, -24.94769321807935825 ) ) ;
#1085 = CARTESIAN_POINT ( 'NONE',  ( 20.69999999999998508, 13.62011893735971135, 86.15790661882942914 ) ) ;
#1086 = LINE ( 'NONE', #2158, #7277 ) ;
#1087 = CARTESIAN_POINT ( 'NONE',  ( 30.07500000054622546, 13.80429023900056507, 95.29460816699764791 ) ) ;
#1088 = VERTEX_POINT ( 'NONE', #6960 ) ;
#1089 = EDGE_CURVE ( 'NONE', #6104, #315, #2142, .T. ) ;
#1090 = DIRECTION ( 'NONE',  ( -1.000000000000000000, -0.000000000000000000, -0.000000000000000000 ) ) ;
#1091 = ORIENTED_EDGE ( 'NONE', *, *, #12423, .T. ) ;
#1092 = CARTESIAN_POINT ( 'NONE',  ( 6.000000000000000000, 5.839897972853064445, -8.673617379884035472E-15 ) ) ;
#1093 = ORIENTED_EDGE ( 'NONE', *, *, #3973, .F. ) ;
#1094 = AXIS2_PLACEMENT_3D ( 'NONE', #536, #2312, #8215 ) ;
#1095 = FACE_OUTER_BOUND ( 'NONE', #9405, .T. ) ;
#1096 =( GEOMETRIC_REPRESENTATION_CONTEXT ( 3 ) GLOBAL_UNCERTAINTY_ASSIGNED_CONTEXT ( ( #6777 ) ) GLOBAL_UNIT_ASSIGNED_CONTEXT ( ( #2294, #11170, #6348 ) ) REPRESENTATION_CONTEXT ( 'NONE', 'WORKASPACE' ) );
#1097 = CARTESIAN_POINT ( 'NONE',  ( 27.49999999999999645, 20.00000000000000355, 189.9999999999999716 ) ) ;
#1098 = CARTESIAN_POINT ( 'NONE',  ( 36.47500000054622404, 13.07298590277314432, 88.54243821818161564 ) ) ;
#1099 = DIRECTION ( 'NONE',  ( 0.000000000000000000, -1.000000000000000000, -0.000000000000000000 ) ) ;
#1100 = CARTESIAN_POINT ( 'NONE',  ( 19.75000000109246301, 17.56310227825320425, 98.29316153445363113 ) ) ;
#1101 = CARTESIAN_POINT ( 'NONE',  ( 37.67500000054621978, 24.28113015263587116, 96.68563167572563088 ) ) ;
#1102 = CARTESIAN_POINT ( 'NONE',  ( 43.29999999999999716, 26.37988106264029398, 86.15790661882942914 ) ) ;
#1103 = CARTESIAN_POINT ( 'NONE',  ( 39.19999999999998153, 24.40838939219355197, 84.72553407664153724 ) ) ;
#1104 = DIRECTION ( 'NONE',  ( 1.224646799147353207E-16, 1.000000000000000000, -0.000000000000000000 ) ) ;
#1105 = ORIENTED_EDGE ( 'NONE', *, *, #10705, .T. ) ;
#1106 = AXIS2_PLACEMENT_3D ( 'NONE', #12286, #5873, #10807 ) ;
#1107 = EDGE_CURVE ( 'NONE', #3445, #2882, #3166, .T. ) ;
#1108 = CARTESIAN_POINT ( 'NONE',  ( 32.05000000109247082, 12.86707612778636012, 93.11078899226572503 ) ) ;
#1109 = CARTESIAN_POINT ( 'NONE',  ( 4.491542451266983704, 47.77873343313099497, -24.59354576118897739 ) ) ;
#1110 = EDGE_LOOP ( 'NONE', ( #11355, #6664, #6554, #8560 ) ) ;
#1111 = EDGE_LOOP ( 'NONE', ( #6272, #2199 ) ) ;
#1112 = CARTESIAN_POINT ( 'NONE',  ( 8.979016783829413484, 15.54942851740142729, 26.52260613434120984 ) ) ;
#1113 = ADVANCED_FACE ( 'NONE', ( #9378 ), #5191, .F. ) ;
#1114 = DIRECTION ( 'NONE',  ( 1.000000000000000000, 0.000000000000000000, 0.000000000000000000 ) ) ;
#1115 = AXIS2_PLACEMENT_3D ( 'NONE', #11557, #8638, #1781 ) ;
#1116 = DIRECTION ( 'NONE',  ( -1.000000000000000000, -0.000000000000000000, -0.000000000000000000 ) ) ;
#1117 = CARTESIAN_POINT ( 'NONE',  ( 34.87500000054623683, 22.36655054427230382, 83.50966788445364841 ) ) ;
#1118 = CARTESIAN_POINT ( 'NONE',  ( 31.67500000054622333, 24.28113015263587116, 96.68563167572563088 ) ) ;
#1119 = DIRECTION ( 'NONE',  ( -1.000000000000000000, -0.000000000000000000, -0.000000000000000000 ) ) ;
#1120 = EDGE_CURVE ( 'NONE', #1690, #3559, #7466, .T. ) ;
#1121 = CARTESIAN_POINT ( 'NONE',  ( 9.741722118349221304, 22.28203113172896366, -26.25078299423969952 ) ) ;
#1122 = CARTESIAN_POINT ( 'NONE',  ( 27.49999999999999645, 20.00000000000000355, 172.0000000000000000 ) ) ;
#1123 = EDGE_LOOP ( 'NONE', ( #4739, #11937, #4393, #7054, #11382, #5372 ) ) ;
#1124 = CARTESIAN_POINT ( 'NONE',  ( 48.87500000054622262, 20.00000000000000355, 83.50966788445364841 ) ) ;
#1125 = CARTESIAN_POINT ( 'NONE',  ( 4.999999999999999112, 50.32998418051842293, -24.49489742783177348 ) ) ;
#1126 = CARTESIAN_POINT ( 'NONE',  ( 0.000000000000000000, -3.000000000000003109, 0.000000000000000000 ) ) ;
#1127 = VERTEX_POINT ( 'NONE', #7402 ) ;
#1128 = PLANE ( 'NONE',  #8232 ) ;
#1129 = VECTOR ( 'NONE', #1119, 1000.000000000000000 ) ;
#1130 = ORIENTED_EDGE ( 'NONE', *, *, #3730, .T. ) ;
#1131 = CARTESIAN_POINT ( 'NONE',  ( 0.000000000000000000, -2.342598717236902051, 4.057500000000004547 ) ) ;
#1132 = ORIENTED_EDGE ( 'NONE', *, *, #3887, .T. ) ;
#1133 = CYLINDRICAL_SURFACE ( 'NONE', #4793, 25.00000000000000000 ) ;
#1134 = EDGE_CURVE ( 'NONE', #2251, #8953, #680, .T. ) ;
#1135 = DIRECTION ( 'NONE',  ( 0.000000000000000000, 1.000000000000000000, 0.000000000000000000 ) ) ;
#1136 = CARTESIAN_POINT ( 'NONE',  ( 23.99529484836403626, 27.49999999999999645, 148.5047051516359318 ) ) ;
#1137 = CARTESIAN_POINT ( 'NONE',  ( 121.9999999999999858, 0.000000000000000000, 5.035999999999999588 ) ) ;
#1138 = CARTESIAN_POINT ( 'NONE',  ( 9.477187959615639201, 23.25714206674319939, 18.74197276232252563 ) ) ;
#1139 = DIRECTION ( 'NONE',  ( -1.000000000000000000, -0.000000000000000000, -0.000000000000000000 ) ) ;
#1140 = DIRECTION ( 'NONE',  ( 0.000000000000000000, 1.000000000000000000, -1.224646799147353207E-16 ) ) ;
#1141 = CARTESIAN_POINT ( 'NONE',  ( 44.87500000054623683, 22.36655054427230382, 83.50966788445364841 ) ) ;
#1142 = CARTESIAN_POINT ( 'NONE',  ( 8.667518415056527203, 14.97026592263945410, 23.45254893740142066 ) ) ;
#1143 = ORIENTED_EDGE ( 'NONE', *, *, #10775, .T. ) ;
#1144 = CARTESIAN_POINT ( 'NONE',  ( 9.658351069856484727, 22.61227114741398836, -23.05920763558311037 ) ) ;
#1145 = VECTOR ( 'NONE', #11967, 1000.000000000000000 ) ;
#1146 = ADVANCED_FACE ( 'NONE', ( #4546 ), #8482, .F. ) ;
#1147 = PRODUCT_CONTEXT ( 'NONE', #8453, 'mechanical' ) ;
#1148 = CARTESIAN_POINT ( 'NONE',  ( 20.97500000054622049, 22.36655054427230382, 83.50966788445364841 ) ) ;
#1149 = CARTESIAN_POINT ( 'NONE',  ( 27.49999999999999645, 20.00000000000000355, 189.9999999999999716 ) ) ;
#1150 = CARTESIAN_POINT ( 'NONE',  ( 32.27500000054622831, 12.34168156654572357, 90.79316153445363113 ) ) ;
#1151 =( BOUNDED_CURVE ( )  B_SPLINE_CURVE ( 2, ( #11518, #9500, #4799, #3842, #1745, #739, #862, #2643, #2704, #10562, #9376 ),
 .UNSPECIFIED., .F., .F. ) 
 B_SPLINE_CURVE_WITH_KNOTS ( ( 3, 2, 2, 2, 2, 3 ),
 ( 0.03333333333333336063, 0.04000000000000003553, 0.04666666666666670349, 0.05333333333333337839, 0.06000000000000005329, 0.06666666666666672125 ),
 .UNSPECIFIED. ) 
 CURVE ( )  GEOMETRIC_REPRESENTATION_ITEM ( )  RATIONAL_B_SPLINE_CURVE ( ( 0.9999999999999998890, 0.9510565162951537532, 1.000000000000000000, 0.9510565162951535312, 1.000000000000000000, 0.9510565162951535312, 1.000000000000000000, 0.9510565162951535312, 1.000000000000000000, 0.9510565162951530871, 1.000000000000000444 ) ) 
 REPRESENTATION_ITEM ( '' )  );
#1152 = CARTESIAN_POINT ( 'NONE',  ( 0.3289161358670515400, 10.00000000000000355, -25.00000000000000711 ) ) ;
#1153 = CARTESIAN_POINT ( 'NONE',  ( 22.29999999999999005, 13.62011893735971135, 95.42841645007781892 ) ) ;
#1154 = DIRECTION ( 'NONE',  ( 1.000000000000000000, -0.000000000000000000, -0.000000000000000000 ) ) ;
#1155 = CARTESIAN_POINT ( 'NONE',  ( 36.27500000054623541, 12.34168156654572535, 90.79316153445363113 ) ) ;
#1156 = ORIENTED_EDGE ( 'NONE', *, *, #5948, .T. ) ;
#1157 = FACE_OUTER_BOUND ( 'NONE', #5042, .T. ) ;
#1158 = SURFACE_SIDE_STYLE ('',( #8652 ) ) ;
#1159 = VERTEX_POINT ( 'NONE', #8360 ) ;
#1160 = CARTESIAN_POINT ( 'NONE',  ( 48.85000000109246088, 24.40838939219355197, 84.72553407664153724 ) ) ;
#1161 = ORIENTED_EDGE ( 'NONE', *, *, #1432, .F. ) ;
#1162 = VECTOR ( 'NONE', #6011, 1000.000000000000000 ) ;
#1163 = DIRECTION ( 'NONE',  ( 1.000000000000000000, -0.000000000000000000, 0.000000000000000000 ) ) ;
#1164 = CARTESIAN_POINT ( 'NONE',  ( 19.99999999999999645, 20.00000000000000355, 189.9999999999999716 ) ) ;
#1165 = CARTESIAN_POINT ( 'NONE',  ( 36.17500000054622689, 13.80429023900056507, 95.29460816699764791 ) ) ;
#1166 = CARTESIAN_POINT ( 'NONE',  ( 40.05000000109246372, 12.86707612778636012, 93.11078899226572503 ) ) ;
#1167 = EDGE_CURVE ( 'NONE', #1407, #9685, #1532, .T. ) ;
#1168 = CARTESIAN_POINT ( 'NONE',  ( 49.37500000054622973, 26.92701409722686634, 93.04388485072563242 ) ) ;
#1169 = CARTESIAN_POINT ( 'NONE',  ( 40.77500000054622831, 17.63344945572770328, 83.50966788445364841 ) ) ;
#1170 = CARTESIAN_POINT ( 'NONE',  ( 41.19999999999998863, 24.40838939219355197, 84.72553407664153724 ) ) ;
#1171 = AXIS2_PLACEMENT_3D ( 'NONE', #2713, #7729, #5763 ) ;
#1172 = CARTESIAN_POINT ( 'NONE',  ( 12.59999999999999964, 7.347880794884118750E-16, -5.999999999999999112 ) ) ;
#1173 = EDGE_LOOP ( 'NONE', ( #10670, #4078, #770, #3547 ) ) ;
#1174 = EDGE_CURVE ( 'NONE', #8715, #3634, #892, .T. ) ;
#1175 = CARTESIAN_POINT ( 'NONE',  ( 28.15000000109246159, 12.11403331821300533, 90.79316153445363113 ) ) ;
#1176 = CARTESIAN_POINT ( 'NONE',  ( 2.065847364689658683, 45.44381439048179772, -24.91495664786098274 ) ) ;
#1177 = ORIENTED_EDGE ( 'NONE', *, *, #1850, .T. ) ;
#1178 = ORIENTED_EDGE ( 'NONE', *, *, #6560, .F. ) ;
#1179 = CARTESIAN_POINT ( 'NONE',  ( 25.15000000109246159, 27.88596668178699645, 90.79316153445363113 ) ) ;
#1180 = VECTOR ( 'NONE', #4602, 1000.000000000000000 ) ;
#1181 = CARTESIAN_POINT ( 'NONE',  ( 6.000000000000000000, 2.919948986426538884, 5.057499999999996554 ) ) ;
#1182 = DIRECTION ( 'NONE',  ( 0.000000000000000000, 0.000000000000000000, -1.000000000000000000 ) ) ;
#1183 = CARTESIAN_POINT ( 'NONE',  ( 28.57500000054622902, 15.71886984736413773, 84.90069139318163138 ) ) ;
#1184 = CARTESIAN_POINT ( 'NONE',  ( 30.87500000054622618, 20.00000000000000355, 83.50966788445364841 ) ) ;
#1185 = CARTESIAN_POINT ( 'NONE',  ( -2.505388173364745175, 54.33011157738807384, 27.88806253468715468 ) ) ;
#1186 = CYLINDRICAL_SURFACE ( 'NONE', #5029, 7.500000000000000000 ) ;
#1187 = AXIS2_PLACEMENT_3D ( 'NONE', #3900, #7778, #2956 ) ;
#1188 = ORIENTED_EDGE ( 'NONE', *, *, #5383, .T. ) ;
#1189 = EDGE_CURVE ( 'NONE', #5465, #2989, #8238, .T. ) ;
#1190 = CARTESIAN_POINT ( 'NONE',  ( 49.45000000109246940, 24.40838939219354842, 96.86078899226572503 ) ) ;
#1191 = ORIENTED_EDGE ( 'NONE', *, *, #7359, .F. ) ;
#1192 = ORIENTED_EDGE ( 'NONE', *, *, #9696, .T. ) ;
#1193 = FACE_BOUND ( 'NONE', #3685, .T. ) ;
#1194 = CARTESIAN_POINT ( 'NONE',  ( -4.146974088394097535, 10.89458658634673327, -24.65552811365946440 ) ) ;
#1195 = EDGE_CURVE ( 'NONE', #12457, #8906, #10198, .T. ) ;
#1196 = EDGE_CURVE ( 'NONE', #6710, #2612, #4774, .T. ) ;
#1197 = VECTOR ( 'NONE', #6338, 1000.000000000000000 ) ;
#1198 = CARTESIAN_POINT ( 'NONE',  ( 0.000000000000000000, 20.00000000000000355, 109.9999999999999858 ) ) ;
#1199 = DIRECTION ( 'NONE',  ( 0.000000000000000000, 0.000000000000000000, 1.000000000000000000 ) ) ;
#1200 = CARTESIAN_POINT ( 'NONE',  ( 8.865759858943656369, 24.63049972072609961, 84.88850774032545132 ) ) ;
#1201 = CARTESIAN_POINT ( 'NONE',  ( 2.644456282953588921, 45.75339465611970269, -24.86012065554512063 ) ) ;
#1202 = CARTESIAN_POINT ( 'NONE',  ( 8.957304208062865314, 24.45789625178892734, 18.99462261546309705 ) ) ;
#1203 = CARTESIAN_POINT ( 'NONE',  ( 6.000000000000000000, 2.919948986426526005, -5.057500000000003659 ) ) ;
#1204 = CARTESIAN_POINT ( 'NONE',  ( -4.332262076698200737, 47.49833309567487305, 27.66292863318953366 ) ) ;
#1205 = AXIS2_PLACEMENT_3D ( 'NONE', #8995, #2139, #308 ) ;
#1206 = CARTESIAN_POINT ( 'NONE',  ( 20.27158385259951956, 18.00000000000000355, 152.2284161474004520 ) ) ;
#1207 = EDGE_LOOP ( 'NONE', ( #11253, #4786, #1003, #11710 ) ) ;
#1208 = AXIS2_PLACEMENT_3D ( 'NONE', #31, #11575, #11640 ) ;
#1209 = CARTESIAN_POINT ( 'NONE',  ( 27.49999999999999645, 20.00000000000000355, 189.9999999999999716 ) ) ;
#1210 = PRODUCT_CONTEXT ( 'NONE', #7562, 'mechanical' ) ;
#1211 = AXIS2_PLACEMENT_3D ( 'NONE', #3932, #10461, #4763 ) ;
#1212 = CARTESIAN_POINT ( 'NONE',  ( 23.17500000054622333, 26.19570976099943849, 86.29171490190961435 ) ) ;
#1213 = CARTESIAN_POINT ( 'NONE',  ( 49.87500000054622262, 20.00000000000000355, 98.07665518445361386 ) ) ;
#1214 = CARTESIAN_POINT ( 'NONE',  ( 31.77500000054622831, 20.00000000000000355, 98.07665518445361386 ) ) ;
#1215 = CARTESIAN_POINT ( 'NONE',  ( 23.47500000054622404, 26.92701409722686634, 93.04388485072563242 ) ) ;
#1216 = CARTESIAN_POINT ( 'NONE',  ( 21.19999999999998508, 24.40838939219355197, 84.72553407664153724 ) ) ;
#1217 = CARTESIAN_POINT ( 'NONE',  ( -2.000000000000015543, 20.00000000000000355, 90.79316153445363113 ) ) ;
#1218 = CARTESIAN_POINT ( 'NONE',  ( 28.77500000054622831, 20.00000000000000355, 83.50966788445364841 ) ) ;
#1219 = ORIENTED_EDGE ( 'NONE', *, *, #5683, .F. ) ;
#1220 = CARTESIAN_POINT ( 'NONE',  ( 23.25000000109246656, 27.13292387221364876, 93.11078899226573924 ) ) ;
#1221 = VERTEX_POINT ( 'NONE', #7338 ) ;
#1222 = DIRECTION ( 'NONE',  ( -1.000000000000000000, -0.000000000000000000, -0.000000000000000000 ) ) ;
#1223 = VERTEX_POINT ( 'NONE', #11206 ) ;
#1224 = DIRECTION ( 'NONE',  ( 0.000000000000000000, 0.000000000000000000, 1.000000000000000000 ) ) ;
#1225 = CARTESIAN_POINT ( 'NONE',  ( 35.47500000054622404, 26.92701409722686634, 93.04388485072563242 ) ) ;
#1226 = DIRECTION ( 'NONE',  ( -0.7071067811865469066, 0.000000000000000000, -0.7071067811865482389 ) ) ;
#1227 = CARTESIAN_POINT ( 'NONE',  ( 39.27500000054622831, 26.92701409722686634, 88.54243821818162985 ) ) ;
#1228 = CARTESIAN_POINT ( 'NONE',  ( 41.29999999999999716, 26.37988106264029398, 86.15790661882942914 ) ) ;
#1229 = ADVANCED_FACE ( 'NONE', ( #2519 ), #10255, .F. ) ;
#1230 = CARTESIAN_POINT ( 'NONE',  ( 48.97500000054622404, 24.28113015263587471, 84.90069139318163138 ) ) ;
#1231 = EDGE_LOOP ( 'NONE', ( #11800, #2663, #6478, #8732 ) ) ;
#1232 = CARTESIAN_POINT ( 'NONE',  ( 30.05000000109246727, 12.86707612778636012, 93.11078899226572503 ) ) ;
#1233 = CARTESIAN_POINT ( 'NONE',  ( -3.246935905771412667, 10.51876153604172970, 24.79592758899451255 ) ) ;
#1234 = ORIENTED_EDGE ( 'NONE', *, *, #5145, .F. ) ;
#1235 = LINE ( 'NONE', #3713, #430 ) ;
#1236 = ORIENTED_EDGE ( 'NONE', *, *, #4278, .T. ) ;
#1237 = VECTOR ( 'NONE', #4254, 1000.000000000000000 ) ;
#1238 = CARTESIAN_POINT ( 'NONE',  ( 6.000000000000000000, -4.379923479639802331, -2.528749999999991616 ) ) ;
#1239 = CARTESIAN_POINT ( 'NONE',  ( 6.000000000000000000, 0.000000000000000000, 0.000000000000000000 ) ) ;
#1240 = LINE ( 'NONE', #4151, #2913 ) ;
#1241 = CARTESIAN_POINT ( 'NONE',  ( 32.27500000054622831, 12.34168156654572535, 90.79316153445363113 ) ) ;
#1242 = CARTESIAN_POINT ( 'NONE',  ( 28.87500000054622262, 20.00000000000000355, 83.50966788445364841 ) ) ;
#1243 = CARTESIAN_POINT ( 'NONE',  ( 43.85000000109246798, 15.59161060780645691, 96.86078899226572503 ) ) ;
#1244 = FACE_OUTER_BOUND ( 'NONE', #7078, .T. ) ;
#1245 = ORIENTED_EDGE ( 'NONE', *, *, #6971, .T. ) ;
#1246 = AXIS2_PLACEMENT_3D ( 'NONE', #11104, #3428, #2411 ) ;
#1247 = CARTESIAN_POINT ( 'NONE',  ( 47.67500000054622689, 24.28113015263587116, 96.68563167572563088 ) ) ;
#1248 = CARTESIAN_POINT ( 'NONE',  ( 49.05000000109246372, 27.13292387221364876, 88.47553407664153724 ) ) ;
#1249 = CARTESIAN_POINT ( 'NONE',  ( -27.49999999999999645, 20.00000000000000355, 99.99999999999997158 ) ) ;
#1250 = ORIENTED_EDGE ( 'NONE', *, *, #11960, .T. ) ;
#1251 = CARTESIAN_POINT ( 'NONE',  ( -36.00000000000000711, 81.39339828220178674, 154.3533255156881694 ) ) ;
#1252 = ADVANCED_FACE ( 'NONE', ( #3777 ), #6759, .F. ) ;
#1253 = ORIENTED_EDGE ( 'NONE', *, *, #10753, .F. ) ;
#1254 = CARTESIAN_POINT ( 'NONE',  ( -4.158535434072708092, 10.89987024370912572, -20.58639742492232827 ) ) ;
#1255 = DIRECTION ( 'NONE',  ( -0.000000000000000000, 0.000000000000000000, 1.000000000000000000 ) ) ;
#1256 = CARTESIAN_POINT ( 'NONE',  ( 2.217963917954424602, 54.49304390046189894, 24.90325875173717662 ) ) ;
#1257 = CARTESIAN_POINT ( 'NONE',  ( 8.561724788085411930, 25.17060510151400976, 85.35530319090553064 ) ) ;
#1258 = DIRECTION ( 'NONE',  ( 0.000000000000000000, 0.000000000000000000, -1.000000000000000000 ) ) ;
#1259 = CARTESIAN_POINT ( 'NONE',  ( 2.630514865864268970, 29.67066479083239372, 20.84486189436999837 ) ) ;
#1260 = CARTESIAN_POINT ( 'NONE',  ( 3.975399702753076525, 46.95009918027220408, -20.62111044216656452 ) ) ;
#1261 = CARTESIAN_POINT ( 'NONE',  ( -50.00000000000001421, 92.00000000000000000, 166.8533255156881694 ) ) ;
#1262 = EDGE_CURVE ( 'NONE', #8484, #223, #865, .T. ) ;
#1263 = CARTESIAN_POINT ( 'NONE',  ( 43.77500000054622831, 20.00000000000000355, 98.07665518445361386 ) ) ;
#1264 = LINE ( 'NONE', #4178, #9947 ) ;
#1265 = ORIENTED_EDGE ( 'NONE', *, *, #2271, .T. ) ;
#1266 = B_SPLINE_CURVE_WITH_KNOTS ( 'NONE', 3,
 ( #4749, #8741, #6707, #55, #8495, #2843, #5641, #3668, #10576, #1887, #1260, #9763, #1072, #5952, #10828, #9827, #6896, #11726, #183, #10761 ),
 .UNSPECIFIED., .F., .F.,
 ( 4, 2, 2, 2, 2, 2, 2, 2, 2, 4 ),
 ( 0.01568878760782931384, 0.01666929802245319808, 0.01764980843707708580, 0.01863031885170097005, 0.01961082926632485429, 0.02059133968094873854, 0.02157185009557262279, 0.02255236051019651050, 0.02304261571750846130, 0.02353287092482041556 ),
 .UNSPECIFIED. ) ;
#1267 = CARTESIAN_POINT ( 'NONE',  ( -4.486434092443181143, 52.21331568334087336, 24.59426911350885092 ) ) ;
#1268 =( BOUNDED_CURVE ( )  B_SPLINE_CURVE ( 2, ( #6445, #1569, #3524, #11021, #5442, #9313, #11268, #9061, #8108, #11978, #9122 ),
 .UNSPECIFIED., .F., .F. ) 
 B_SPLINE_CURVE_WITH_KNOTS ( ( 3, 2, 2, 2, 2, 3 ),
 ( 0.3666666666666666963, 0.3733333333333334059, 0.3800000000000000600, 0.3866666666666667695, 0.3933333333333334236, 0.4000000000000001332 ),
 .UNSPECIFIED. ) 
 CURVE ( )  GEOMETRIC_REPRESENTATION_ITEM ( )  RATIONAL_B_SPLINE_CURVE ( ( 0.9999999999999995559, 0.9510565162951539753, 1.000000000000000000, 0.9510565162951535312, 1.000000000000000000, 0.9510565162951535312, 1.000000000000000000, 0.9510565162951535312, 1.000000000000000000, 0.9510565162951527540, 1.000000000000000888 ) ) 
 REPRESENTATION_ITEM ( '' )  );
#1269 = EDGE_CURVE ( 'NONE', #11196, #1420, #9006, .T. ) ;
#1270 = CARTESIAN_POINT ( 'NONE',  ( 20.17500000054622333, 13.80429023900056507, 95.29460816699764791 ) ) ;
#1271 = CARTESIAN_POINT ( 'NONE',  ( 46.97500000054621694, 22.36655054427230382, 83.50966788445364841 ) ) ;
#1272 = CARTESIAN_POINT ( 'NONE',  ( 33.57500000054623257, 24.28113015263587116, 96.68563167572563088 ) ) ;
#1273 = CARTESIAN_POINT ( 'NONE',  ( 20.57500000054622546, 13.80429023900056684, 86.29171490190961435 ) ) ;
#1274 = DIRECTION ( 'NONE',  ( 1.000000000000000000, -0.000000000000000000, -0.000000000000000000 ) ) ;
#1275 = CARTESIAN_POINT ( 'NONE',  ( -111.8465843842649292, 77.00000000000000000, 94.35332551568819781 ) ) ;
#1276 = CARTESIAN_POINT ( 'NONE',  ( 28.37500000054622618, 13.07298590277314432, 88.54243821818161564 ) ) ;
#1277 = ORIENTED_EDGE ( 'NONE', *, *, #10927, .F. ) ;
#1278 = CARTESIAN_POINT ( 'NONE',  ( 32.95000000109246230, 26.37988106264029398, 86.15790661882942914 ) ) ;
#1279 = VERTEX_POINT ( 'NONE', #11653 ) ;
#1280 = ORIENTED_EDGE ( 'NONE', *, *, #3433, .T. ) ;
#1281 = CARTESIAN_POINT ( 'NONE',  ( 49.93750000027311131, 20.00000000000000355, 98.18490835945361539 ) ) ;
#1282 = ORIENTED_EDGE ( 'NONE', *, *, #4134, .T. ) ;
#1283 =( NAMED_UNIT ( * ) PLANE_ANGLE_UNIT ( ) SI_UNIT ( $, .RADIAN. ) );
#1284 = CARTESIAN_POINT ( 'NONE',  ( 0.000000000000000000, 20.00000000000000355, -28.00000000000000711 ) ) ;
#1285 = AXIS2_PLACEMENT_3D ( 'NONE', #4758, #11420, #5533 ) ;
#1286 = CARTESIAN_POINT ( 'NONE',  ( 40.17500000054622689, 13.80429023900056507, 95.29460816699764791 ) ) ;
#1287 = CARTESIAN_POINT ( 'NONE',  ( -1.619441697059012419, 54.74165912786163801, -27.95475164937197121 ) ) ;
#1288 = CARTESIAN_POINT ( 'NONE',  ( 19.85000000109246443, 15.59161060780645691, 96.86078899226572503 ) ) ;
#1289 = CARTESIAN_POINT ( 'NONE',  ( 40.87500000054622262, 20.00000000000000355, 83.50966788445364841 ) ) ;
#1290 = CARTESIAN_POINT ( 'NONE',  ( 41.99999999999998579, 20.00000000000000355, 98.29316153445363113 ) ) ;
#1291 = CARTESIAN_POINT ( 'NONE',  ( 44.47500000054622404, 13.80429023900056684, 86.29171490190961435 ) ) ;
#1292 = VERTEX_POINT ( 'NONE', #11460 ) ;
#1293 = CIRCLE ( 'NONE', #9192, 5.000000000000000888 ) ;
#1294 = CARTESIAN_POINT ( 'NONE',  ( 26.45000000109246585, 15.59161060780646046, 84.72553407664153724 ) ) ;
#1295 = DIRECTION ( 'NONE',  ( -0.7071067811865502373, 8.659560562354966138E-17, 0.7071067811865449082 ) ) ;
#1296 = ORIENTED_EDGE ( 'NONE', *, *, #6893, .T. ) ;
#1297 = CARTESIAN_POINT ( 'NONE',  ( 1.302738838705299829, 54.83847614797452508, -20.96203534374045674 ) ) ;
#1298 = CARTESIAN_POINT ( 'NONE',  ( 26.37500000054622618, 12.34168156654572357, 90.79316153445363113 ) ) ;
#1299 = ORIENTED_EDGE ( 'NONE', *, *, #9071, .F. ) ;
#1300 = ADVANCED_FACE ( 'NONE', ( #12475 ), #11868, .T. ) ;
#1301 = CARTESIAN_POINT ( 'NONE',  ( 25.25000000109246301, 27.13292387221364876, 93.11078899226573924 ) ) ;
#1302 = CARTESIAN_POINT ( 'NONE',  ( 41.35000000109245377, 26.37988106264029398, 95.42841645007781892 ) ) ;
#1303 = EDGE_CURVE ( 'NONE', #5355, #12320, #3557, .T. ) ;
#1304 = CARTESIAN_POINT ( 'NONE',  ( 48.69999999999998153, 13.62011893735970958, 86.15790661882942914 ) ) ;
#1305 = CIRCLE ( 'NONE', #4943, 26.49999999999999645 ) ;
#1306 = CARTESIAN_POINT ( 'NONE',  ( 32.17500000054622689, 13.07298590277314254, 93.04388485072563242 ) ) ;
#1307 = CARTESIAN_POINT ( 'NONE',  ( 32.67500000054622689, 15.71886984736413773, 84.90069139318163138 ) ) ;
#1308 = AXIS2_PLACEMENT_3D ( 'NONE', #4527, #11251, #10481 ) ;
#1309 = CARTESIAN_POINT ( 'NONE',  ( -50.00000000000001421, 20.00000000000000000, 145.0000000000000000 ) ) ;
#1310 = CARTESIAN_POINT ( 'NONE',  ( 27.49999999999999645, 20.00000000000000355, 170.0000000000000000 ) ) ;
#1311 = CARTESIAN_POINT ( 'NONE',  ( 22.25000000109246656, 12.86707612778636012, 88.47553407664152303 ) ) ;
#1312 = ORIENTED_EDGE ( 'NONE', *, *, #12502, .F. ) ;
#1313 = CARTESIAN_POINT ( 'NONE',  ( 46.95000000109246940, 26.37988106264029398, 86.15790661882942914 ) ) ;
#1314 = SURFACE_STYLE_USAGE ( .BOTH. , #484 ) ;
#1315 = ORIENTED_EDGE ( 'NONE', *, *, #5224, .F. ) ;
#1316 = LINE ( 'NONE', #8101, #1145 ) ;
#1317 = VERTEX_POINT ( 'NONE', #7783 ) ;
#1318 = AXIS2_PLACEMENT_3D ( 'NONE', #6837, #7793, #11665 ) ;
#1319 = CARTESIAN_POINT ( 'NONE',  ( -6.116903510341333394, 12.06222645458920084, -20.09722343790940613 ) ) ;
#1320 = CARTESIAN_POINT ( 'NONE',  ( 0.000000000000000000, -2.919948986426523341, 5.057500000000002771 ) ) ;
#1321 = ADVANCED_FACE ( 'NONE', ( #10437, #3845 ), #12353, .T. ) ;
#1322 = CARTESIAN_POINT ( 'NONE',  ( -8.658175568303594360, 14.98574592473889311, 23.45342671841680371 ) ) ;
#1323 = CARTESIAN_POINT ( 'NONE',  ( 22.79999999999998650, 15.59161060780646046, 84.72553407664153724 ) ) ;
#1324 = CARTESIAN_POINT ( 'NONE',  ( -3.050580840359966128, 46.02510565206127779, -24.81467268664276560 ) ) ;
#1325 = LINE ( 'NONE', #4174, #9796 ) ;
#1326 = CARTESIAN_POINT ( 'NONE',  ( -1.295685194009021490, 45.16801400859229432, 27.97044664692164773 ) ) ;
#1327 = PRODUCT_RELATED_PRODUCT_CATEGORY ( 'part', '', ( #6786 ) ) ;
#1328 = APPLICATION_CONTEXT ( 'automotive_design' ) ;
#1329 = CARTESIAN_POINT ( 'NONE',  ( 44.17500000054622689, 13.07298590277314254, 93.04388485072563242 ) ) ;
#1330 = ADVANCED_FACE ( 'NONE', ( #6825 ), #9644, .T. ) ;
#1331 = DIRECTION ( 'NONE',  ( 0.000000000000000000, 0.000000000000000000, 1.000000000000000000 ) ) ;
#1332 = VERTEX_POINT ( 'NONE', #1064 ) ;
#1333 = CARTESIAN_POINT ( 'NONE',  ( -8.488101409370928607, 14.70313273146787836, -26.68309740503542571 ) ) ;
#1334 = ITEM_DEFINED_TRANSFORMATION ( 'NONE', 'NONE', #12036,  #9021 ) ;
#1335 = DIRECTION ( 'NONE',  ( -1.000000000000000000, 0.000000000000000000, 0.000000000000000000 ) ) ;
#1336 = CARTESIAN_POINT ( 'NONE',  ( 46.57500000054623257, 13.80429023900056684, 86.29171490190961435 ) ) ;
#1337 = CARTESIAN_POINT ( 'NONE',  ( 30.67500000054622689, 17.63344945572770328, 83.50966788445364841 ) ) ;
#1338 = CARTESIAN_POINT ( 'NONE',  ( 20.27500000054622475, 13.07298590277314254, 93.04388485072563242 ) ) ;
#1339 = CARTESIAN_POINT ( 'NONE',  ( -2.000000000000015543, 20.00000000000000355, 83.29316153445364534 ) ) ;
#1340 = VECTOR ( 'NONE', #10577, 1000.000000000000000 ) ;
#1341 = FACE_OUTER_BOUND ( 'NONE', #9704, .T. ) ;
#1342 = CARTESIAN_POINT ( 'NONE',  ( 25.37500000054622973, 26.92701409722686634, 93.04388485072563242 ) ) ;
#1343 = ORIENTED_EDGE ( 'NONE', *, *, #11108, .T. ) ;
#1344 = EDGE_CURVE ( 'NONE', #9751, #10006, #4573, .T. ) ;
#1345 = VECTOR ( 'NONE', #9054, 1000.000000000000114 ) ;
#1346 = LINE ( 'NONE', #11289, #1826 ) ;
#1347 = VERTEX_POINT ( 'NONE', #2706 ) ;
#1348 = VERTEX_POINT ( 'NONE', #10624 ) ;
#1349 = CARTESIAN_POINT ( 'NONE',  ( 27.49999999999999645, 20.00000000000000355, 197.9999999999999716 ) ) ;
#1350 = EDGE_LOOP ( 'NONE', ( #3303, #487, #9055, #3936, #12305, #464 ) ) ;
#1351 = CARTESIAN_POINT ( 'NONE',  ( 0.000000000000000000, 0.000000000000000000, 0.000000000000000000 ) ) ;
#1352 = EDGE_CURVE ( 'NONE', #11822, #3847, #7629, .T. ) ;
#1353 = CARTESIAN_POINT ( 'NONE',  ( 36.07500000054622546, 15.71886984736413417, 96.68563167572563088 ) ) ;
#1354 = CARTESIAN_POINT ( 'NONE',  ( 36.89999999999999147, 17.56310227825322912, 83.29316153445363113 ) ) ;
#1355 = CARTESIAN_POINT ( 'NONE',  ( -2.000000000000015543, 20.00000000000000355, 90.79316153445363113 ) ) ;
#1356 = CARTESIAN_POINT ( 'NONE',  ( 40.37500000054621552, 12.34168156654572535, 90.79316153445363113 ) ) ;
#1357 = CARTESIAN_POINT ( 'NONE',  ( 36.19999999999998863, 15.59161060780645691, 96.86078899226572503 ) ) ;
#1358 = CARTESIAN_POINT ( 'NONE',  ( 44.17500000054622689, 13.07298590277314254, 93.04388485072563242 ) ) ;
#1359 = VERTEX_POINT ( 'NONE', #5629 ) ;
#1360 = CARTESIAN_POINT ( 'NONE',  ( 26.85000000109246443, 24.40838939219355197, 84.72553407664153724 ) ) ;
#1361 = DIRECTION ( 'NONE',  ( -1.000000000000000000, -0.000000000000000000, -0.000000000000000000 ) ) ;
#1362 = CIRCLE ( 'NONE', #11078, 6.599999999999999645 ) ;
#1363 = ORIENTED_EDGE ( 'NONE', *, *, #3044, .T. ) ;
#1364 = CARTESIAN_POINT ( 'NONE',  ( -10.00000000000000355, 20.00000000000000355, 26.15339366124404208 ) ) ;
#1365 = ORIENTED_EDGE ( 'NONE', *, *, #1416, .F. ) ;
#1366 = CARTESIAN_POINT ( 'NONE',  ( 3.237495866348039986, 10.53285331842846340, 27.81400203867760368 ) ) ;
#1367 = CARTESIAN_POINT ( 'NONE',  ( 4.999999999999999112, 49.67322169183177039, -27.54995462791183769 ) ) ;
#1368 = DIRECTION ( 'NONE',  ( 0.000000000000000000, 0.000000000000000000, 1.000000000000000000 ) ) ;
#1369 = AXIS2_PLACEMENT_3D ( 'NONE', #9446, #1818, #6703 ) ;
#1370 = CARTESIAN_POINT ( 'NONE',  ( 29.47500000054622404, 26.19570976099943493, 95.29460816699764791 ) ) ;
#1371 = CARTESIAN_POINT ( 'NONE',  ( 25.77500000054622831, 22.36655054427230027, 98.07665518445361386 ) ) ;
#1372 = CARTESIAN_POINT ( 'NONE',  ( 1.311921753209796648, 29.93550986204568787, 27.97677076635717341 ) ) ;
#1373 = DIRECTION ( 'NONE',  ( 0.000000000000000000, 0.000000000000000000, 1.000000000000000000 ) ) ;
#1374 = ORIENTED_EDGE ( 'NONE', *, *, #12157, .T. ) ;
#1375 = CARTESIAN_POINT ( 'NONE',  ( 43.45000000109246230, 24.40838939219354842, 96.86078899226572503 ) ) ;
#1376 = ORIENTED_EDGE ( 'NONE', *, *, #2334, .F. ) ;
#1377 = LINE ( 'NONE', #11841, #2958 ) ;
#1378 = ORIENTED_EDGE ( 'NONE', *, *, #7422, .T. ) ;
#1379 = CIRCLE ( 'NONE', #5423, 4.057500000000000107 ) ;
#1380 = CARTESIAN_POINT ( 'NONE',  ( -7.294862588765995248, 13.15250477205630553, -19.69373592174549259 ) ) ;
#1381 = LINE ( 'NONE', #12218, #5021 ) ;
#1382 = CARTESIAN_POINT ( 'NONE',  ( 20.07500000054622546, 13.80429023900056507, 95.29460816699764791 ) ) ;
#1383 = SURFACE_STYLE_USAGE ( .BOTH. , #1503 ) ;
#1384 = DIRECTION ( 'NONE',  ( 0.000000000000000000, 0.000000000000000000, 1.000000000000000000 ) ) ;
#1385 = CARTESIAN_POINT ( 'NONE',  ( 22.49999999999998934, 12.11403331821300533, 90.79316153445363113 ) ) ;
#1386 = CYLINDRICAL_SURFACE ( 'NONE', #3731, 28.00000000000000355 ) ;
#1387 = CARTESIAN_POINT ( 'NONE',  ( -9.869687208716547033, 18.35727153228636155, 26.20294053744295937 ) ) ;
#1388 = EDGE_CURVE ( 'NONE', #2031, #9944, #805, .T. ) ;
#1389 = CARTESIAN_POINT ( 'NONE',  ( -4.968290342600433007, 49.34811171367579163, 27.55576829111012316 ) ) ;
#1390 = CARTESIAN_POINT ( 'NONE',  ( -0.6585108229100932187, 45.03273675766970285, -24.99339394906690970 ) ) ;
#1391 = ORIENTED_EDGE ( 'NONE', *, *, #2650, .F. ) ;
#1392 = AXIS2_PLACEMENT_3D ( 'NONE', #5200, #9007, #7217 ) ;
#1393 = CARTESIAN_POINT ( 'NONE',  ( 3.061565168526138680E-15, 55.00000000000000000, 25.00000000000000000 ) ) ;
#1394 = EDGE_CURVE ( 'NONE', #9622, #8859, #7003, .T. ) ;
#1395 =( GEOMETRIC_REPRESENTATION_CONTEXT ( 3 ) GLOBAL_UNCERTAINTY_ASSIGNED_CONTEXT ( ( #9754 ) ) GLOBAL_UNIT_ASSIGNED_CONTEXT ( ( #11010, #11965, #8161 ) ) REPRESENTATION_CONTEXT ( 'NONE', 'WORKASPACE' ) );
#1396 = CARTESIAN_POINT ( 'NONE',  ( 25.99999999999998934, 20.00000000000000355, 98.29316153445363113 ) ) ;
#1397 = CYLINDRICAL_SURFACE ( 'NONE', #947, 10.00000000000000355 ) ;
#1398 = CARTESIAN_POINT ( 'NONE',  ( 42.97500000054622404, 22.36655054427230382, 83.50966788445364841 ) ) ;
#1399 = EDGE_CURVE ( 'NONE', #11822, #707, #1556, .T. ) ;
#1400 = CARTESIAN_POINT ( 'NONE',  ( 24.77500000054622831, 20.00000000000000355, 83.50966788445364841 ) ) ;
#1401 = VECTOR ( 'NONE', #11784, 1000.000000000000000 ) ;
#1402 = CARTESIAN_POINT ( 'NONE',  ( 9.868114579493717287, 18.34823788458374594, -22.97009550651098309 ) ) ;
#1403 = LINE ( 'NONE', #1339, #9996 ) ;
#1404 = DIRECTION ( 'NONE',  ( 0.000000000000000000, 0.000000000000000000, 1.000000000000000000 ) ) ;
#1405 = CARTESIAN_POINT ( 'NONE',  ( 31.99999999999998579, 20.00000000000000355, 98.29316153445363113 ) ) ;
#1406 = CARTESIAN_POINT ( 'NONE',  ( 26.67500000054622689, 17.63344945572770328, 83.50966788445364841 ) ) ;
#1407 = VERTEX_POINT ( 'NONE', #5698 ) ;
#1408 = DIRECTION ( 'NONE',  ( 1.000000000000000000, -0.000000000000000000, -0.000000000000000000 ) ) ;
#1409 = ORIENTED_EDGE ( 'NONE', *, *, #9208, .F. ) ;
#1410 = CARTESIAN_POINT ( 'NONE',  ( 38.39999999999999147, 12.86707612778636012, 93.11078899226572503 ) ) ;
#1411 = VERTEX_POINT ( 'NONE', #10067 ) ;
#1412 = ADVANCED_FACE ( 'NONE', ( #11714 ), #7907, .F. ) ;
#1413 = AXIS2_PLACEMENT_3D ( 'NONE', #6157, #7998, #9904 ) ;
#1414 = CARTESIAN_POINT ( 'NONE',  ( 33.67500000054622689, 24.28113015263587116, 96.68563167572563088 ) ) ;
#1415 = CARTESIAN_POINT ( 'NONE',  ( -3.766645289650884632, 53.30424666614836582, -27.74645978028278392 ) ) ;
#1416 = EDGE_CURVE ( 'NONE', #5416, #3740, #10814, .T. ) ;
#1417 = CARTESIAN_POINT ( 'NONE',  ( 43.37500000054622973, 26.92701409722686634, 93.04388485072563242 ) ) ;
#1418 = CARTESIAN_POINT ( 'NONE',  ( 33.79999999999999005, 24.40838939219354842, 96.86078899226572503 ) ) ;
#1419 = CARTESIAN_POINT ( 'NONE',  ( 45.27500000054622831, 27.65831843345427998, 90.79316153445363113 ) ) ;
#1420 = VERTEX_POINT ( 'NONE', #10005 ) ;
#1421 = CARTESIAN_POINT ( 'NONE',  ( 25.75000000109246301, 17.56310227825320425, 98.29316153445363113 ) ) ;
#1422 = CARTESIAN_POINT ( 'NONE',  ( -9.673562854105167474, 17.38029584746389133, 23.05303382818504332 ) ) ;
#1423 = ORIENTED_EDGE ( 'NONE', *, *, #2963, .T. ) ;
#1424 = EDGE_CURVE ( 'NONE', #8002, #7325, #4223, .T. ) ;
#1425 = CARTESIAN_POINT ( 'NONE',  ( -2.000000000000015543, 20.00000000000000355, 90.79316153445363113 ) ) ;
#1426 = VERTEX_POINT ( 'NONE', #6191 ) ;
#1427 = CYLINDRICAL_SURFACE ( 'NONE', #10025, 9.000000000000000000 ) ;
#1428 = CARTESIAN_POINT ( 'NONE',  ( 20.85000000109246443, 24.40838939219355197, 84.72553407664153724 ) ) ;
#1429 = CARTESIAN_POINT ( 'NONE',  ( 34.99999999999999289, 20.00000000000000355, 171.0000000000000000 ) ) ;
#1430 = VECTOR ( 'NONE', #5911, 999.9999999999998863 ) ;
#1431 = CARTESIAN_POINT ( 'NONE',  ( 24.99999999999998579, 20.00000000000000355, 83.29316153445364534 ) ) ;
#1432 = EDGE_CURVE ( 'NONE', #4353, #9941, #10643, .T. ) ;
#1433 = CARTESIAN_POINT ( 'NONE',  ( 23.47500000054623115, 26.19570976099943493, 95.29460816699764791 ) ) ;
#1434 = CARTESIAN_POINT ( 'NONE',  ( 25.07500000054622191, 24.28113015263587471, 84.90069139318163138 ) ) ;
#1435 = CARTESIAN_POINT ( 'NONE',  ( 6.000000000000000000, 5.839897972853065333, -6.938893903907228378E-15 ) ) ;
#1436 = CARTESIAN_POINT ( 'NONE',  ( 21.65000000109246514, 20.00000000000000355, 98.29316153445363113 ) ) ;
#1437 = EDGE_LOOP ( 'NONE', ( #2533, #1177, #7690, #11506, #832, #5613, #11042, #9817, #1192 ) ) ;
#1438 = CARTESIAN_POINT ( 'NONE',  ( 42.65000000109246514, 20.00000000000000355, 83.29316153445364534 ) ) ;
#1439 = CARTESIAN_POINT ( 'NONE',  ( 5.000000000000000000, -2.342598717236902051, 4.057500000000004547 ) ) ;
#1440 = ORIENTED_EDGE ( 'NONE', *, *, #3266, .F. ) ;
#1441 = DIRECTION ( 'NONE',  ( -0.000000000000000000, -1.000000000000000000, -0.000000000000000000 ) ) ;
#1442 = AXIS2_PLACEMENT_3D ( 'NONE', #2014, #7796, #2975 ) ;
#1443 = ORIENTED_EDGE ( 'NONE', *, *, #5948, .F. ) ;
#1444 = CARTESIAN_POINT ( 'NONE',  ( -3.558434346354896416, 10.64888650799004033, -20.69856808805790038 ) ) ;
#1445 = FACE_OUTER_BOUND ( 'NONE', #2596, .T. ) ;
#1446 = TOROIDAL_SURFACE ( 'NONE', #12378, 13.85889894354065355, 10.00000000000000000 ) ;
#1447 =( NAMED_UNIT ( * ) SI_UNIT ( $, .STERADIAN. ) SOLID_ANGLE_UNIT ( ) );
#1448 = CARTESIAN_POINT ( 'NONE',  ( 0.6000000000000033085, 0.000000000000000000, 0.000000000000000000 ) ) ;
#1449 = CARTESIAN_POINT ( 'NONE',  ( 22.29999999999998295, 13.62011893735970958, 95.42841645007781892 ) ) ;
#1450 = CARTESIAN_POINT ( 'NONE',  ( -9.463516830393745138, 16.75202061662974273, 18.74709386869566430 ) ) ;
#1451 = LINE ( 'NONE', #10077, #8378 ) ;
#1452 = CARTESIAN_POINT ( 'NONE',  ( 4.999999999999999112, -3.000000000000002665, 121.2488769092545198 ) ) ;
#1453 = CARTESIAN_POINT ( 'NONE',  ( -4.245899883333350111, 47.35448134532762055, -24.63697916171703994 ) ) ;
#1454 = ORIENTED_EDGE ( 'NONE', *, *, #8944, .F. ) ;
#1455 = VECTOR ( 'NONE', #6408, 1000.000000000000000 ) ;
#1456 = FACE_OUTER_BOUND ( 'NONE', #11072, .T. ) ;
#1457 = DIRECTION ( 'NONE',  ( 0.000000000000000000, 0.000000000000000000, 1.000000000000000000 ) ) ;
#1458 = EDGE_CURVE ( 'NONE', #7136, #637, #1377, .T. ) ;
#1459 = CARTESIAN_POINT ( 'NONE',  ( 49.71250000081935383, 20.00000000000000355, 98.18490835945361539 ) ) ;
#1460 = CARTESIAN_POINT ( 'NONE',  ( 41.47500000054623115, 26.92701409722686634, 93.04388485072563242 ) ) ;
#1461 = CARTESIAN_POINT ( 'NONE',  ( 24.07500000054622902, 13.80429023900056507, 95.29460816699764791 ) ) ;
#1462 = CARTESIAN_POINT ( 'NONE',  ( 7.146477089513696868, 13.00393516148637651, 88.07960685825688074 ) ) ;
#1463 = CARTESIAN_POINT ( 'NONE',  ( -50.00000000000001421, 0.000000000000000000, 69.99999999999998579 ) ) ;
#1464 = CARTESIAN_POINT ( 'NONE',  ( -50.00000000000001421, 55.00000000000000000, 147.8533255156883399 ) ) ;
#1465 =( NAMED_UNIT ( * ) SI_UNIT ( $, .STERADIAN. ) SOLID_ANGLE_UNIT ( ) );
#1466 = EDGE_LOOP ( 'NONE', ( #3319, #10629, #3956, #11590, #9721, #3647, #7782, #8853, #9846 ) ) ;
#1467 = CARTESIAN_POINT ( 'NONE',  ( 12.59999999999999964, 0.000000000000000000, -6.599999999999998757 ) ) ;
#1468 = EDGE_LOOP ( 'NONE', ( #3196, #7902 ) ) ;
#1469 = CARTESIAN_POINT ( 'NONE',  ( 32.27500000054622831, 13.07298590277314254, 93.04388485072563242 ) ) ;
#1470 = DIRECTION ( 'NONE',  ( 1.000000000000000000, -0.000000000000000000, -0.000000000000000000 ) ) ;
#1471 = CARTESIAN_POINT ( 'NONE',  ( 45.57500000054622546, 24.28113015263587116, 96.68563167572563088 ) ) ;
#1472 = CARTESIAN_POINT ( 'NONE',  ( 32.17500000054621978, 13.80429023900056507, 95.29460816699764791 ) ) ;
#1473 = CARTESIAN_POINT ( 'NONE',  ( 38.29999999999997584, 13.62011893735971135, 95.42841645007781892 ) ) ;
#1474 = EDGE_CURVE ( 'NONE', #10, #3463, #8986, .T. ) ;
#1475 = CARTESIAN_POINT ( 'NONE',  ( 45.87500000054622973, 17.63344945572769973, 98.07665518445361386 ) ) ;
#1476 = ORIENTED_EDGE ( 'NONE', *, *, #1195, .T. ) ;
#1477 = CARTESIAN_POINT ( 'NONE',  ( 26.05000000109246727, 12.86707612778636012, 93.11078899226572503 ) ) ;
#1478 = CARTESIAN_POINT ( 'NONE',  ( -9.481487189274945493, 16.75591109918640242, 23.13382230614692148 ) ) ;
#1479 = ORIENTED_EDGE ( 'NONE', *, *, #4810, .F. ) ;
#1480 = DIRECTION ( 'NONE',  ( 0.000000000000000000, 0.000000000000000000, 1.000000000000000000 ) ) ;
#1481 = ORIENTED_EDGE ( 'NONE', *, *, #5689, .T. ) ;
#1482 = VECTOR ( 'NONE', #5857, 1000.000000000000000 ) ;
#1483 = CARTESIAN_POINT ( 'NONE',  ( -31.74999999999995737, 0.000000000000000000, 0.000000000000000000 ) ) ;
#1484 = LINE ( 'NONE', #10234, #11131 ) ;
#1485 = DIRECTION ( 'NONE',  ( -1.000000000000000000, -0.000000000000000000, -0.000000000000000000 ) ) ;
#1486 = CARTESIAN_POINT ( 'NONE',  ( 25.17500000054623044, 26.92701409722686634, 88.54243821818162985 ) ) ;
#1487 = CARTESIAN_POINT ( 'NONE',  ( 24.97500000054622049, 22.36655054427230382, 83.50966788445364841 ) ) ;
#1488 = AXIS2_PLACEMENT_3D ( 'NONE', #10254, #5256, #5445 ) ;
#1489 = CARTESIAN_POINT ( 'NONE',  ( 4.445126667670568743, 28.98136467921717241, 27.65156766125397070 ) ) ;
#1490 = LINE ( 'NONE', #8220, #10288 ) ;
#1491 = EDGE_LOOP ( 'NONE', ( #541, #9972, #12260, #5849, #3995 ) ) ;
#1492 = CARTESIAN_POINT ( 'NONE',  ( 46.65000000109246514, 20.00000000000000355, 83.29316153445364534 ) ) ;
#1493 = CARTESIAN_POINT ( 'NONE',  ( 5.000000000000000000, 50.00000000000000000, -24.49489742783178414 ) ) ;
#1494 = ORIENTED_EDGE ( 'NONE', *, *, #7603, .F. ) ;
#1495 = CARTESIAN_POINT ( 'NONE',  ( -20.27158385259951956, 18.00000000000000355, 170.0000119999999697 ) ) ;
#1496 = EDGE_CURVE ( 'NONE', #4128, #3442, #11672, .T. ) ;
#1497 = ORIENTED_EDGE ( 'NONE', *, *, #1029, .F. ) ;
#1498 = CARTESIAN_POINT ( 'NONE',  ( -4.441326820874226478, 11.03441940688963108, -24.60408056175351987 ) ) ;
#1499 = AXIS2_PLACEMENT_3D ( 'NONE', #12513, #9480, #8642 ) ;
#1500 = CARTESIAN_POINT ( 'NONE',  ( -9.103371648737914157, 24.15160165414906857, 23.28405058525132176 ) ) ;
#1501 = AXIS2_PLACEMENT_3D ( 'NONE', #7613, #7486, #6647 ) ;
#1502 = EDGE_CURVE ( 'NONE', #4660, #1936, #364, .T. ) ;
#1503 = SURFACE_SIDE_STYLE ('',( #6198 ) ) ;
#1504 = DIRECTION ( 'NONE',  ( 0.000000000000000000, 0.000000000000000000, -1.000000000000000000 ) ) ;
#1505 = DIRECTION ( 'NONE',  ( 0.000000000000000000, 0.4999999999999987232, -0.8660254037844393737 ) ) ;
#1506 = CARTESIAN_POINT ( 'NONE',  ( -8.488010075893786421, 14.70289628708776242, 19.20917730135813528 ) ) ;
#1507 = DIRECTION ( 'NONE',  ( -1.000000000000000000, -0.000000000000000000, -0.000000000000000000 ) ) ;
#1508 = DIRECTION ( 'NONE',  ( -0.000000000000000000, 1.000000000000000000, -0.000000000000000000 ) ) ;
#1509 = AXIS2_PLACEMENT_3D ( 'NONE', #9809, #11901, #3012 ) ;
#1510 = CARTESIAN_POINT ( 'NONE',  ( 23.79999999999998650, 24.40838939219354842, 96.86078899226572503 ) ) ;
#1511 = EDGE_LOOP ( 'NONE', ( #11700, #4285, #649, #5260, #9716 ) ) ;
#1512 = DIRECTION ( 'NONE',  ( 0.000000000000000000, 0.000000000000000000, -1.000000000000000000 ) ) ;
#1513 = AXIS2_PLACEMENT_3D ( 'NONE', #7542, #1014, #10511 ) ;
#1514 = CARTESIAN_POINT ( 'NONE',  ( 3.298734236876446957, 53.76100060739371145, 24.78173945428942204 ) ) ;
#1515 = CARTESIAN_POINT ( 'NONE',  ( 42.27500000054622120, 13.07298590277314254, 93.04388485072563242 ) ) ;
#1516 = CARTESIAN_POINT ( 'NONE',  ( 27.87500000054622618, 17.63344945572769973, 98.07665518445361386 ) ) ;
#1517 = CARTESIAN_POINT ( 'NONE',  ( 9.480548647978427113, 16.81007977654359919, 84.00085956564031164 ) ) ;
#1518 = DIRECTION ( 'NONE',  ( -0.7071067811865460184, -0.000000000000000000, 0.7071067811865490160 ) ) ;
#1519 = LINE ( 'NONE', #9268, #7372 ) ;
#1520 = FACE_OUTER_BOUND ( 'NONE', #5559, .T. ) ;
#1521 = VERTEX_POINT ( 'NONE', #6886 ) ;
#1522 = DIRECTION ( 'NONE',  ( 0.000000000000000000, 0.000000000000000000, -1.000000000000000000 ) ) ;
#1523 = EDGE_LOOP ( 'NONE', ( #7715, #1363 ) ) ;
#1524 = EDGE_CURVE ( 'NONE', #3004, #6574, #1316, .T. ) ;
#1525 = FACE_OUTER_BOUND ( 'NONE', #6316, .T. ) ;
#1526 = VECTOR ( 'NONE', #11390, 1000.000000000000000 ) ;
#1527 = ORIENTED_EDGE ( 'NONE', *, *, #3186, .F. ) ;
#1528 = SHAPE_REPRESENTATION_RELATIONSHIP ( 'NONE' , 'NONE' ,  #10815, #4292 ) ;
#1529 = AXIS2_PLACEMENT_3D ( 'NONE', #7516, #10550, #10487 ) ;
#1530 = CARTESIAN_POINT ( 'NONE',  ( 34.27500000054622120, 13.07298590277314254, 93.04388485072563242 ) ) ;
#1531 = CARTESIAN_POINT ( 'NONE',  ( -5.000000000000000000, 50.00000000000000000, -27.54995462791182703 ) ) ;
#1532 = CIRCLE ( 'NONE', #6197, 10.00000000000000888 ) ;
#1533 = CARTESIAN_POINT ( 'NONE',  ( 43.17500000054622689, 26.92701409722686634, 88.54243821818162985 ) ) ;
#1534 = CARTESIAN_POINT ( 'NONE',  ( 36.17500000054623399, 13.80429023900056507, 95.29460816699764791 ) ) ;
#1535 = CARTESIAN_POINT ( 'NONE',  ( 35.79999999999998295, 24.40838939219354842, 96.86078899226572503 ) ) ;
#1536 = AXIS2_PLACEMENT_3D ( 'NONE', #5941, #8037, #8854 ) ;
#1537 = CARTESIAN_POINT ( 'NONE',  ( 1.313665803496629980, 29.93556061881280428, 24.97400592093060112 ) ) ;
#1538 = CARTESIAN_POINT ( 'NONE',  ( 42.37500000054622262, 13.07298590277314432, 88.54243821818161564 ) ) ;
#1539 = ORIENTED_EDGE ( 'NONE', *, *, #7218, .F. ) ;
#1540 = CARTESIAN_POINT ( 'NONE',  ( 25.25000000109246301, 27.13292387221364876, 93.11078899226573924 ) ) ;
#1541 = CARTESIAN_POINT ( 'NONE',  ( -7.945999201647152788, 13.89399703635140249, 23.70671076423498391 ) ) ;
#1542 = ORIENTED_EDGE ( 'NONE', *, *, #1432, .T. ) ;
#1543 = CARTESIAN_POINT ( 'NONE',  ( -10.00000000000000355, 20.00000000000000355, -26.15339366124404563 ) ) ;
#1544 = ORIENTED_EDGE ( 'NONE', *, *, #11378, .T. ) ;
#1545 = CYLINDRICAL_SURFACE ( 'NONE', #2118, 7.499999999999992895 ) ;
#1546 = DIRECTION ( 'NONE',  ( 0.000000000000000000, 0.000000000000000000, -1.000000000000000000 ) ) ;
#1547 = ADVANCED_FACE ( 'NONE', ( #6007 ), #10954, .F. ) ;
#1548 = AXIS2_PLACEMENT_3D ( 'NONE', #608, #10188, #9117 ) ;
#1549 = DIRECTION ( 'NONE',  ( 1.000000000000000000, -0.000000000000000000, -0.000000000000000000 ) ) ;
#1550 = CARTESIAN_POINT ( 'NONE',  ( 25.69999999999998153, 26.37988106264029398, 95.42841645007781892 ) ) ;
#1551 = CARTESIAN_POINT ( 'NONE',  ( 22.57500000054622902, 15.71886984736413773, 84.90069139318163138 ) ) ;
#1552 = CARTESIAN_POINT ( 'NONE',  ( 26.17500000054622689, 13.80429023900056507, 95.29460816699764791 ) ) ;
#1553 = EDGE_CURVE ( 'NONE', #6911, #6345, #11267, .T. ) ;
#1554 = VECTOR ( 'NONE', #244, 1000.000000000000000 ) ;
#1555 = PLANE ( 'NONE',  #5563 ) ;
#1556 =( BOUNDED_CURVE ( )  B_SPLINE_CURVE ( 3, ( #9627, #935, #4993, #3145 ),
 .UNSPECIFIED., .F., .F. ) 
 B_SPLINE_CURVE_WITH_KNOTS ( ( 4, 4 ),
 ( 1.570796326794896558, 3.141592653589793560 ),
 .UNSPECIFIED. ) 
 CURVE ( )  GEOMETRIC_REPRESENTATION_ITEM ( )  RATIONAL_B_SPLINE_CURVE ( ( 1.000000000000000000, 0.8047378541243649375, 0.8047378541243649375, 1.000000000000000000 ) ) 
 REPRESENTATION_ITEM ( '' )  );
#1557 = CARTESIAN_POINT ( 'NONE',  ( 0.000000000000000000, -3.000000000000003109, 0.000000000000000000 ) ) ;
#1558 = ORIENTED_EDGE ( 'NONE', *, *, #10326, .F. ) ;
#1559 = CARTESIAN_POINT ( 'NONE',  ( 46.25000000109246656, 12.86707612778636012, 88.47553407664152303 ) ) ;
#1560 = VERTEX_POINT ( 'NONE', #7137 ) ;
#1561 = CARTESIAN_POINT ( 'NONE',  ( 12.00000000000000355, 0.000000000000000000, 0.000000000000000000 ) ) ;
#1562 = ORIENTED_EDGE ( 'NONE', *, *, #7766, .T. ) ;
#1563 = DIRECTION ( 'NONE',  ( -0.000000000000000000, -1.000000000000000000, -0.000000000000000000 ) ) ;
#1564 = VECTOR ( 'NONE', #2331, 1000.000000000000000 ) ;
#1565 = CARTESIAN_POINT ( 'NONE',  ( 8.486510062750307171, 14.70060591898896618, -23.51628241912814588 ) ) ;
#1566 = APPLICATION_CONTEXT ( 'automotive_design' ) ;
#1567 = CARTESIAN_POINT ( 'NONE',  ( 29.79999999999998650, 24.40838939219354842, 96.86078899226572503 ) ) ;
#1568 = EDGE_CURVE ( 'NONE', #3396, #2741, #2022, .T. ) ;
#1569 = CARTESIAN_POINT ( 'NONE',  ( 38.55000000109247082, 17.56310227825319359, 83.29316153445364534 ) ) ;
#1570 = DIRECTION ( 'NONE',  ( 0.000000000000000000, -0.8660254037844392627, -0.4999999999999990008 ) ) ;
#1571 = CARTESIAN_POINT ( 'NONE',  ( -50.00000000000001421, 20.00000000000000000, 145.0000000000000000 ) ) ;
#1572 = DIRECTION ( 'NONE',  ( 0.000000000000000000, 0.000000000000000000, 1.000000000000000000 ) ) ;
#1573 = CARTESIAN_POINT ( 'NONE',  ( 47.25000000109246656, 27.13292387221364876, 93.11078899226573924 ) ) ;
#1574 = ORIENTED_EDGE ( 'NONE', *, *, #1120, .F. ) ;
#1575 = EDGE_CURVE ( 'NONE', #9559, #11430, #8792, .T. ) ;
#1576 = CARTESIAN_POINT ( 'NONE',  ( -34.99999999999999289, 20.00000000000000355, 99.99999999999997158 ) ) ;
#1577 = DIRECTION ( 'NONE',  ( 0.000000000000000000, 0.000000000000000000, -1.000000000000000000 ) ) ;
#1578 = CARTESIAN_POINT ( 'NONE',  ( 40.27500000054622120, 13.07298590277314254, 93.04388485072563242 ) ) ;
#1579 = CARTESIAN_POINT ( 'NONE',  ( 27.57500000054622902, 24.28113015263587116, 96.68563167572563088 ) ) ;
#1580 = CARTESIAN_POINT ( 'NONE',  ( 6.688794870772565737, 12.56618450651110308, 89.76590532369878872 ) ) ;
#1581 = CARTESIAN_POINT ( 'NONE',  ( 4.491750101222253377, 47.77928715861156661, 24.59350609687774281 ) ) ;
#1582 = CARTESIAN_POINT ( 'NONE',  ( 5.000000000000000000, -2.342598717236902051, 4.057500000000004547 ) ) ;
#1583 = PLANE ( 'NONE',  #12145 ) ;
#1584 = AXIS2_PLACEMENT_3D ( 'NONE', #1209, #6901, #8873 ) ;
#1585 = VERTEX_POINT ( 'NONE', #3081 ) ;
#1586 = DIRECTION ( 'NONE',  ( 1.224646799147353207E-16, 1.000000000000000000, 0.000000000000000000 ) ) ;
#1587 = ORIENTED_EDGE ( 'NONE', *, *, #2660, .T. ) ;
#1588 = CARTESIAN_POINT ( 'NONE',  ( 6.000000000000000000, 0.000000000000000000, 0.000000000000000000 ) ) ;
#1589 = AXIS2_PLACEMENT_3D ( 'NONE', #944, #3788, #3720 ) ;
#1590 = CARTESIAN_POINT ( 'NONE',  ( 29.97500000054622404, 17.63344945572769973, 98.07665518445361386 ) ) ;
#1591 = CARTESIAN_POINT ( 'NONE',  ( 27.55000000109246017, 22.43689772174679575, 98.29316153445363113 ) ) ;
#1592 = CARTESIAN_POINT ( 'NONE',  ( 47.17500000054623399, 26.92701409722686634, 88.54243821818162985 ) ) ;
#1593 = AXIS2_PLACEMENT_3D ( 'NONE', #10131, #1441, #4352 ) ;
#1594 = CARTESIAN_POINT ( 'NONE',  ( 31.87500000054622262, 20.00000000000000355, 98.07665518445361386 ) ) ;
#1595 = CARTESIAN_POINT ( 'NONE',  ( 36.39999999999999147, 12.86707612778636012, 93.11078899226572503 ) ) ;
#1596 = LINE ( 'NONE', #10278, #4640 ) ;
#1597 = CARTESIAN_POINT ( 'NONE',  ( 38.37500000054622973, 13.07298590277314432, 88.54243821818161564 ) ) ;
#1598 = EDGE_LOOP ( 'NONE', ( #3810, #5059 ) ) ;
#1599 = CARTESIAN_POINT ( 'NONE',  ( 49.17500000054622689, 26.92701409722686634, 88.54243821818162985 ) ) ;
#1600 = CARTESIAN_POINT ( 'NONE',  ( -1.614021781250221999, 45.25640150583762988, -20.94007668992154692 ) ) ;
#1601 = EDGE_LOOP ( 'NONE', ( #10052, #6468, #11504, #299, #2507, #758 ) ) ;
#1602 = CARTESIAN_POINT ( 'NONE',  ( -3.543284028218923964, 29.35697078463959642, -27.77658592395861703 ) ) ;
#1603 = VERTEX_POINT ( 'NONE', #10751 ) ;
#1604 =( NAMED_UNIT ( * ) PLANE_ANGLE_UNIT ( ) SI_UNIT ( $, .RADIAN. ) );
#1605 = VECTOR ( 'NONE', #11075, 1000.000000000000114 ) ;
#1606 = CARTESIAN_POINT ( 'NONE',  ( 21.05000000109246727, 27.13292387221364876, 88.47553407664153724 ) ) ;
#1607 = FACE_BOUND ( 'NONE', #1601, .T. ) ;
#1608 = CARTESIAN_POINT ( 'NONE',  ( 0.000000000000000000, 5.839897972853064445, -8.673617379884035472E-15 ) ) ;
#1609 = ADVANCED_FACE ( 'NONE', ( #2063 ), #1128, .T. ) ;
#1610 = CARTESIAN_POINT ( 'NONE',  ( 23.97500000054623115, 15.71886984736413417, 96.68563167572563088 ) ) ;
#1611 = CARTESIAN_POINT ( 'NONE',  ( 24.57500000054622191, 13.80429023900056684, 86.29171490190961435 ) ) ;
#1612 = CARTESIAN_POINT ( 'NONE',  ( 6.000000000000000000, 0.000000000000000000, 0.000000000000000000 ) ) ;
#1613 = CONICAL_SURFACE ( 'NONE', #603, 25.00000000000000355, 0.7853981633974482790 ) ;
#1614 = CARTESIAN_POINT ( 'NONE',  ( 44.99999999999999289, 20.00000000000000355, 83.29316153445364534 ) ) ;
#1615 = ORIENTED_EDGE ( 'NONE', *, *, #7849, .T. ) ;
#1616 = CARTESIAN_POINT ( 'NONE',  ( 39.55000000109246372, 22.43689772174679575, 98.29316153445363113 ) ) ;
#1617 = ORIENTED_EDGE ( 'NONE', *, *, #9229, .F. ) ;
#1618 = CARTESIAN_POINT ( 'NONE',  ( 30.05000000109246727, 12.86707612778636012, 93.11078899226572503 ) ) ;
#1619 = ORIENTED_EDGE ( 'NONE', *, *, #5676, .F. ) ;
#1620 = DIRECTION ( 'NONE',  ( -0.000000000000000000, -0.000000000000000000, 1.000000000000000000 ) ) ;
#1621 = CARTESIAN_POINT ( 'NONE',  ( 9.105349949761121664, 15.85277269881838258, -23.28327519851026040 ) ) ;
#1622 = CARTESIAN_POINT ( 'NONE',  ( 19.97500000054623115, 15.71886984736413417, 96.68563167572563088 ) ) ;
#1623 =( BOUNDED_CURVE ( )  B_SPLINE_CURVE ( 2, ( #3041, #8876, #8946, #2153, #1894, #4947, #8690, #1081, #62, #8811, #10645 ),
 .UNSPECIFIED., .F., .F. ) 
 B_SPLINE_CURVE_WITH_KNOTS ( ( 3, 2, 2, 2, 2, 3 ),
 ( 0.8333333333333333703, 0.8399999999999999689, 0.8466666666666666785, 0.8533333333333333881, 0.8599999999999999867, 0.8666666666666666963 ),
 .UNSPECIFIED. ) 
 CURVE ( )  GEOMETRIC_REPRESENTATION_ITEM ( )  RATIONAL_B_SPLINE_CURVE ( ( 1.000000000000000000, 0.9510565162951535312, 1.000000000000000000, 0.9510565162951535312, 1.000000000000000000, 0.9510565162951535312, 1.000000000000000000, 0.9510565162951535312, 1.000000000000000000, 0.9510565162951535312, 1.000000000000000000 ) ) 
 REPRESENTATION_ITEM ( '' )  );
#1624 = DIRECTION ( 'NONE',  ( 0.000000000000000000, 0.000000000000000000, 1.000000000000000000 ) ) ;
#1625 = CARTESIAN_POINT ( 'NONE',  ( 27.49999999999998579, 27.88596668178699645, 90.79316153445363113 ) ) ;
#1626=STYLED_ITEM('',(#12584),#2150);
#1627 = EDGE_CURVE ( 'NONE', #58, #10066, #662, .T. ) ;
#1628 = CARTESIAN_POINT ( 'NONE',  ( -7.537341967019228761, 13.39683431484485965, 19.60665308794510864 ) ) ;
#1629 = DIRECTION ( 'NONE',  ( -0.000000000000000000, -0.000000000000000000, -1.000000000000000000 ) ) ;
#1630 = CARTESIAN_POINT ( 'NONE',  ( 26.97500000054622760, 24.28113015263587471, 84.90069139318163138 ) ) ;
#1631 = CARTESIAN_POINT ( 'NONE',  ( 9.916835782772588814, 21.32911185711201796, 22.94902338049798374 ) ) ;
#1632 = CARTESIAN_POINT ( 'NONE',  ( 47.65000000109246514, 20.00000000000000355, 98.29316153445363113 ) ) ;
#1633 = EDGE_LOOP ( 'NONE', ( #1376, #9658, #7352, #7644 ) ) ;
#1634 = DIRECTION ( 'NONE',  ( 0.000000000000000000, 0.000000000000000000, -1.000000000000000000 ) ) ;
#1635 = FACE_OUTER_BOUND ( 'NONE', #1173, .T. ) ;
#1636 = CARTESIAN_POINT ( 'NONE',  ( 39.67500000054623399, 22.36655054427230027, 98.07665518445361386 ) ) ;
#1637 = CARTESIAN_POINT ( 'NONE',  ( 39.27500000054622831, 26.92701409722686634, 88.54243821818162985 ) ) ;
#1638 = CARTESIAN_POINT ( 'NONE',  ( 28.77500000054622831, 20.00000000000000355, 83.50966788445364841 ) ) ;
#1639 = CARTESIAN_POINT ( 'NONE',  ( -27.49999999999999645, 20.00000000000000355, 99.99999999999997158 ) ) ;
#1640 = CARTESIAN_POINT ( 'NONE',  ( 4.839779845606726916, 48.70264860999793655, 24.52714343409649089 ) ) ;
#1641 = EDGE_CURVE ( 'NONE', #1292, #7797, #6003, .T. ) ;
#1642 = CARTESIAN_POINT ( 'NONE',  ( 4.999999999999998224, 18.00000000000000355, 152.2284161474004520 ) ) ;
#1643 = DIRECTION ( 'NONE',  ( -0.000000000000000000, 1.039664082171044875E-15, 1.000000000000000000 ) ) ;
#1644 = ORIENTED_EDGE ( 'NONE', *, *, #6426, .F. ) ;
#1645 = VECTOR ( 'NONE', #9659, 1000.000000000000000 ) ;
#1646 = CARTESIAN_POINT ( 'NONE',  ( 6.000000000000000000, -2.919948986426523341, 5.057500000000002771 ) ) ;
#1647 = ORIENTED_EDGE ( 'NONE', *, *, #1575, .F. ) ;
#1648 = CARTESIAN_POINT ( 'NONE',  ( 6.000000000000000000, -2.919948986426523341, 5.057500000000002771 ) ) ;
#1649 = ADVANCED_FACE ( 'NONE', ( #9304 ), #424, .F. ) ;
#1650 = CARTESIAN_POINT ( 'NONE',  ( 29.67500000054622333, 24.28113015263587116, 96.68563167572563088 ) ) ;
#1651 = CARTESIAN_POINT ( 'NONE',  ( 26.85000000109246443, 24.40838939219355197, 84.72553407664153724 ) ) ;
#1652 = CARTESIAN_POINT ( 'NONE',  ( 48.87500000054622262, 22.36655054427230382, 83.50966788445364841 ) ) ;
#1653 = EDGE_CURVE ( 'NONE', #12416, #3301, #8224, .T. ) ;
#1654 = CARTESIAN_POINT ( 'NONE',  ( 33.77500000054623541, 22.36655054427230027, 98.07665518445361386 ) ) ;
#1655 = CARTESIAN_POINT ( 'NONE',  ( 29.79999999999998650, 24.40838939219354842, 96.86078899226572503 ) ) ;
#1656 = CARTESIAN_POINT ( 'NONE',  ( 8.972329510183547185, 24.46440230363330315, 23.33606587946024291 ) ) ;
#1657 = CARTESIAN_POINT ( 'NONE',  ( 38.17500000054622689, 13.07298590277314254, 93.04388485072563242 ) ) ;
#1658 = ORIENTED_EDGE ( 'NONE', *, *, #1399, .F. ) ;
#1659 = CARTESIAN_POINT ( 'NONE',  ( 20.05000000109246372, 12.86707612778636012, 93.11078899226572503 ) ) ;
#1660 = DIRECTION ( 'NONE',  ( 0.000000000000000000, 0.000000000000000000, 1.000000000000000000 ) ) ;
#1661 = ORIENTED_EDGE ( 'NONE', *, *, #6688, .T. ) ;
#1662 = CARTESIAN_POINT ( 'NONE',  ( 0.000000000000000000, 67.00000000000000000, 0.000000000000000000 ) ) ;
#1663 = ORIENTED_EDGE ( 'NONE', *, *, #10791, .F. ) ;
#1664 = CARTESIAN_POINT ( 'NONE',  ( 5.839560020365381021, 28.12428960229776465, -24.30998564924267313 ) ) ;
#1665 = CARTESIAN_POINT ( 'NONE',  ( 10.00000000000000533, 19.33329863329985443, 26.15339366124404563 ) ) ;
#1666 = PLANE ( 'NONE',  #11498 ) ;
#1667 = DIRECTION ( 'NONE',  ( 0.000000000000000000, 0.000000000000000000, -1.000000000000000000 ) ) ;
#1668 = CARTESIAN_POINT ( 'NONE',  ( 21.67500000054622689, 22.36655054427230027, 98.07665518445361386 ) ) ;
#1669 = CARTESIAN_POINT ( 'NONE',  ( 49.99999999999998579, 20.00000000000000355, 98.29316153445363113 ) ) ;
#1670 = DIRECTION ( 'NONE',  ( 0.000000000000000000, 0.000000000000000000, -1.000000000000000000 ) ) ;
#1671 = DIRECTION ( 'NONE',  ( -1.000000000000000000, 0.000000000000000000, 0.000000000000000000 ) ) ;
#1672 = VERTEX_POINT ( 'NONE', #3461 ) ;
#1673 = CARTESIAN_POINT ( 'NONE',  ( 35.35000000109246798, 26.37988106264029398, 95.42841645007781892 ) ) ;
#1674 = VERTEX_POINT ( 'NONE', #12030 ) ;
#1675 = PLANE ( 'NONE',  #2938 ) ;
#1676 = ORIENTED_EDGE ( 'NONE', *, *, #10874, .T. ) ;
#1677 = EDGE_CURVE ( 'NONE', #2800, #2324, #10246, .T. ) ;
#1678 = CARTESIAN_POINT ( 'NONE',  ( -8.664197377259947430, 14.96499702975700608, -23.45374477514955203 ) ) ;
#1679 = CARTESIAN_POINT ( 'NONE',  ( 10.00000000000000711, 19.66959671226640793, -18.46618531261938756 ) ) ;
#1680 = CARTESIAN_POINT ( 'NONE',  ( -7.930305867179300527, 26.10041404063223780, 23.70984975861344779 ) ) ;
#1681 = VECTOR ( 'NONE', #2476, 1000.000000000000000 ) ;
#1682 = DIRECTION ( 'NONE',  ( 1.000000000000000000, 0.000000000000000000, 0.000000000000000000 ) ) ;
#1683 = CARTESIAN_POINT ( 'NONE',  ( -0.3273843838414227103, 45.00000000000000711, 20.99999999999999645 ) ) ;
#1684 = CARTESIAN_POINT ( 'NONE',  ( 3.767132220643788720, 53.30373896185297866, -27.74639645793992671 ) ) ;
#1685 = CARTESIAN_POINT ( 'NONE',  ( -1.648786683818842080, 10.13141593593141287, 27.95326983821354005 ) ) ;
#1686 = CARTESIAN_POINT ( 'NONE',  ( 21.87500000054622973, 17.63344945572769973, 98.07665518445361386 ) ) ;
#1687 = CARTESIAN_POINT ( 'NONE',  ( 8.972329510183547185, 24.46440230363330315, 23.33606587946024291 ) ) ;
#1688 = CIRCLE ( 'NONE', #1488, 10.00000000000000355 ) ;
#1689 = DIRECTION ( 'NONE',  ( 0.000000000000000000, -0.4999999999999986677, 0.8660254037844392627 ) ) ;
#1690 = VERTEX_POINT ( 'NONE', #7326 ) ;
#1691 = PRODUCT_DEFINITION ( 'UNKNOWN', '', #9398, #9044 ) ;
#1692 = DIRECTION ( 'NONE',  ( 0.000000000000000000, 0.000000000000000000, 1.000000000000000000 ) ) ;
#1693 = EDGE_CURVE ( 'NONE', #9959, #2943, #595, .T. ) ;
#1694 = CARTESIAN_POINT ( 'NONE',  ( 29.65000000109246514, 20.00000000000000355, 98.29316153445363113 ) ) ;
#1695 = CARTESIAN_POINT ( 'NONE',  ( 39.97500000054623115, 17.63344945572769973, 98.07665518445361386 ) ) ;
#1696 = VECTOR ( 'NONE', #4340, 1000.000000000000000 ) ;
#1697 = CARTESIAN_POINT ( 'NONE',  ( 23.27500000054622475, 27.65831843345427998, 90.79316153445363113 ) ) ;
#1698 = CARTESIAN_POINT ( 'NONE',  ( 9.796481954667255465, 17.97777750360451066, 98.01975852014066959 ) ) ;
#1699 = CARTESIAN_POINT ( 'NONE',  ( 2.216120825188211185, 45.50613141711284015, 24.90340997055814398 ) ) ;
#1700 = CIRCLE ( 'NONE', #11843, 9.499999999999994671 ) ;
#1701 = EDGE_CURVE ( 'NONE', #3198, #4057, #5498, .T. ) ;
#1702 = LINE ( 'NONE', #374, #11227 ) ;
#1703 = DIRECTION ( 'NONE',  ( 0.000000000000000000, 0.000000000000000000, 1.000000000000000000 ) ) ;
#1704 = DIRECTION ( 'NONE',  ( 0.000000000000000000, 0.000000000000000000, 1.000000000000000000 ) ) ;
#1705 = ORIENTED_EDGE ( 'NONE', *, *, #12125, .F. ) ;
#1706 = LINE ( 'NONE', #883, #10755 ) ;
#1707 = DIRECTION ( 'NONE',  ( 0.000000000000000000, 0.000000000000000000, -1.000000000000000000 ) ) ;
#1708 = VECTOR ( 'NONE', #10819, 1000.000000000000000 ) ;
#1709 = CARTESIAN_POINT ( 'NONE',  ( 28.27500000054622475, 13.07298590277314254, 93.04388485072563242 ) ) ;
#1710 = CARTESIAN_POINT ( 'NONE',  ( 36.87500000054622973, 22.36655054427230382, 83.50966788445364841 ) ) ;
#1711 = CARTESIAN_POINT ( 'NONE',  ( 25.87500000054622618, 20.00000000000000355, 98.07665518445361386 ) ) ;
#1712 = CARTESIAN_POINT ( 'NONE',  ( 30.09999999999999076, 17.56310227825320425, 98.29316153445363113 ) ) ;
#1713 = EDGE_CURVE ( 'NONE', #9005, #7706, #9367, .T. ) ;
#1714 = CARTESIAN_POINT ( 'NONE',  ( 8.124594680848492345, 25.83911103074633075, 23.64375881965231230 ) ) ;
#1715 = CARTESIAN_POINT ( 'NONE',  ( 42.07500000054623257, 13.80429023900056507, 95.29460816699764791 ) ) ;
#1716 = VERTEX_POINT ( 'NONE', #8163 ) ;
#1717 = PRESENTATION_LAYER_ASSIGNMENT (  '', '', ( #923 ) ) ;
#1718 = CARTESIAN_POINT ( 'NONE',  ( 21.25000000109246301, 27.13292387221364876, 93.11078899226573924 ) ) ;
#1719 = CARTESIAN_POINT ( 'NONE',  ( 27.95000000109246585, 13.62011893735970958, 95.42841645007781892 ) ) ;
#1720 = ORIENTED_EDGE ( 'NONE', *, *, #9869, .T. ) ;
#1721 = APPLICATION_CONTEXT ( 'automotive_design' ) ;
#1722 = CARTESIAN_POINT ( 'NONE',  ( -6.197539731915355238E-14, 9.999999999999182876, 21.00000000000039080 ) ) ;
#1723 = VERTEX_POINT ( 'NONE', #11259 ) ;
#1724 = EDGE_CURVE ( 'NONE', #110, #2004, #4550, .T. ) ;
#1725 = CARTESIAN_POINT ( 'NONE',  ( 5.034037828167091000, 28.66467738801596354, -24.49412005228846922 ) ) ;
#1726 = CARTESIAN_POINT ( 'NONE',  ( 2.000000000000008882, 20.00000000000000711, 169.9999999999999716 ) ) ;
#1727 = DIRECTION ( 'NONE',  ( 0.000000000000000000, 0.000000000000000000, -1.000000000000000000 ) ) ;
#1728 = CARTESIAN_POINT ( 'NONE',  ( 42.77500000054622120, 17.63344945572770328, 83.50966788445364841 ) ) ;
#1729 = CARTESIAN_POINT ( 'NONE',  ( -27.49999999999999645, 20.00000000000000355, 170.0000119999999697 ) ) ;
#1730 = CARTESIAN_POINT ( 'NONE',  ( 43.97500000054622404, 17.63344945572769973, 98.07665518445361386 ) ) ;
#1731 = CARTESIAN_POINT ( 'NONE',  ( 46.29999999999999005, 13.62011893735971135, 95.42841645007781892 ) ) ;
#1732 = CARTESIAN_POINT ( 'NONE',  ( 6.000000000000000000, -2.919948986426525117, 5.057500000000004547 ) ) ;
#1733 = CARTESIAN_POINT ( 'NONE',  ( -3.051014581595654640, 46.02544827001062089, 24.81461801464184802 ) ) ;
#1734 = ORIENTED_EDGE ( 'NONE', *, *, #2101, .T. ) ;
#1735 = CARTESIAN_POINT ( 'NONE',  ( 40.05000000109246372, 12.86707612778636012, 93.11078899226572503 ) ) ;
#1736 = CARTESIAN_POINT ( 'NONE',  ( 1.302929565828678582, 54.83844695853547790, -24.96811105270434439 ) ) ;
#1737 = ORIENTED_EDGE ( 'NONE', *, *, #11608, .T. ) ;
#1738 = ORIENTED_EDGE ( 'NONE', *, *, #2968, .F. ) ;
#1739 = SHAPE_REPRESENTATION ( 'Bearing Block Mounting Shaft', ( #9021 ), #11237 ) ;
#1740 = CARTESIAN_POINT ( 'NONE',  ( 1.659095203930551543, 10.13304969779982301, -20.93688979605049738 ) ) ;
#1741 = CARTESIAN_POINT ( 'NONE',  ( -9.868806730738530320, 21.64797418619996350, 22.96979908047426377 ) ) ;
#1742 = CARTESIAN_POINT ( 'NONE',  ( -31.74999999999995737, 0.000000000000000000, 0.000000000000000000 ) ) ;
#1743 = CARTESIAN_POINT ( 'NONE',  ( 0.000000000000000000, 20.00000000000000355, 109.9999999999999858 ) ) ;
#1744 = DIRECTION ( 'NONE',  ( 0.000000000000000000, -0.000000000000000000, 1.000000000000000000 ) ) ;
#1745 = CARTESIAN_POINT ( 'NONE',  ( 48.25000000109246656, 12.86707612778636012, 88.47553407664152303 ) ) ;
#1746 = CARTESIAN_POINT ( 'NONE',  ( 49.57500000054621836, 26.19570976099943493, 95.29460816699764791 ) ) ;
#1747 = FACE_OUTER_BOUND ( 'NONE', #10984, .T. ) ;
#1748 = VERTEX_POINT ( 'NONE', #6437 ) ;
#1749 = VECTOR ( 'NONE', #7752, 1000.000000000000000 ) ;
#1750 = ORIENTED_EDGE ( 'NONE', *, *, #4293, .F. ) ;
#1751 = CARTESIAN_POINT ( 'NONE',  ( 43.15000000109247225, 27.88596668178699645, 90.79316153445363113 ) ) ;
#1752 = DIRECTION ( 'NONE',  ( -1.000000000000000000, -0.000000000000000000, -0.000000000000000000 ) ) ;
#1753 = CARTESIAN_POINT ( 'NONE',  ( 40.77500000054622831, 17.63344945572770328, 83.50966788445364841 ) ) ;
#1754 = CARTESIAN_POINT ( 'NONE',  ( 22.87500000054622973, 22.36655054427230382, 83.50966788445364841 ) ) ;
#1755 = EDGE_CURVE ( 'NONE', #7072, #3840, #7389, .T. ) ;
#1756 = DIRECTION ( 'NONE',  ( 0.000000000000000000, 0.000000000000000000, 1.000000000000000000 ) ) ;
#1757 = DIRECTION ( 'NONE',  ( 0.000000000000000000, 0.000000000000000000, 1.000000000000000000 ) ) ;
#1758 = CARTESIAN_POINT ( 'NONE',  ( -111.8465843842649292, 84.49999999999998579, 146.8533255156881978 ) ) ;
#1759 = CARTESIAN_POINT ( 'NONE',  ( 0.6550766687392827192, 45.03237040378185441, 27.99416758511093661 ) ) ;
#1760 = CARTESIAN_POINT ( 'NONE',  ( 0.000000000000000000, 0.000000000000000000, 8.400000000000000355 ) ) ;
#1761 = ORIENTED_EDGE ( 'NONE', *, *, #10783, .F. ) ;
#1762 = DIRECTION ( 'NONE',  ( 0.000000000000000000, 0.000000000000000000, 1.000000000000000000 ) ) ;
#1763 = AXIS2_PLACEMENT_3D ( 'NONE', #8719, #2949, #2051 ) ;
#1764 = CARTESIAN_POINT ( 'NONE',  ( 54.99999999999999289, 0.000000000000000000, 379.9999999999999432 ) ) ;
#1765 = EDGE_CURVE ( 'NONE', #10983, #11823, #10301, .T. ) ;
#1766 = CARTESIAN_POINT ( 'NONE',  ( 28.37500000054622262, 12.34168156654572357, 90.79316153445363113 ) ) ;
#1767 = CARTESIAN_POINT ( 'NONE',  ( 29.45000000109246230, 24.40838939219354842, 96.86078899226572503 ) ) ;
#1768 = CARTESIAN_POINT ( 'NONE',  ( 37.17500000054622689, 26.92701409722686634, 88.54243821818162985 ) ) ;
#1769 = CARTESIAN_POINT ( 'NONE',  ( 24.97500000054622049, 22.36655054427230382, 83.50966788445364841 ) ) ;
#1770 = CARTESIAN_POINT ( 'NONE',  ( 31.69999999999999218, 26.37988106264029398, 95.42841645007781892 ) ) ;
#1771 = CARTESIAN_POINT ( 'NONE',  ( 49.99999999999998579, 20.00000000000000355, 98.29316153445363113 ) ) ;
#1772 = CARTESIAN_POINT ( 'NONE',  ( 42.27500000054622831, 12.34168156654572535, 90.79316153445363113 ) ) ;
#1773 = ORIENTED_EDGE ( 'NONE', *, *, #12369, .T. ) ;
#1774 = EDGE_CURVE ( 'NONE', #11133, #10329, #7061, .T. ) ;
#1775 = CARTESIAN_POINT ( 'NONE',  ( 46.77500000054622831, 20.00000000000000355, 83.50966788445364841 ) ) ;
#1776 = CARTESIAN_POINT ( 'NONE',  ( -5.000000000000000888, 49.67263425446288494, -20.39607805437114152 ) ) ;
#1777 = ORIENTED_EDGE ( 'NONE', *, *, #28, .F. ) ;
#1778 = B_SPLINE_CURVE_WITH_KNOTS ( 'NONE', 3,
 ( #9551, #9365, #8407, #9609, #6556, #8526, #9488, #5615, #917, #3576, #8650, #11322, #2629, #7578, #982, #4848, #9798, #6929, #4912, #1918, #8967, #8714, #6871, #3003 ),
 .UNSPECIFIED., .F., .F.,
 ( 4, 2, 2, 2, 2, 2, 2, 2, 2, 2, 2, 4 ),
 ( 0.000000000000000000, 0.001975470015275241145, 0.002963205022912861284, 0.003950940030550481423, 0.005926410045825732976, 0.006914145053463355284, 0.007901880061100976724, 0.009877350076376223073, 0.01185282009165146769, 0.01284055509928909086, 0.01382829010692671404, 0.01580376012220196039 ),
 .UNSPECIFIED. ) ;
#1779 = CARTESIAN_POINT ( 'NONE',  ( 9.737577724063894991, 17.70041058371123555, 18.60604745661291659 ) ) ;
#1780 = ORIENTED_EDGE ( 'NONE', *, *, #11066, .F. ) ;
#1781 = DIRECTION ( 'NONE',  ( 0.000000000000000000, 0.000000000000000000, -1.000000000000000000 ) ) ;
#1782 = AXIS2_PLACEMENT_3D ( 'NONE', #11582, #168, #295 ) ;
#1783 = CARTESIAN_POINT ( 'NONE',  ( 20.00000000000001421, 24.39339828220178674, 137.5000000000000000 ) ) ;
#1784 = ADVANCED_FACE ( 'NONE', ( #6253 ), #5244, .T. ) ;
#1785 = DIRECTION ( 'NONE',  ( -0.5000000000000046629, 1.060575238724903587E-16, -0.8660254037844359321 ) ) ;
#1786 = CARTESIAN_POINT ( 'NONE',  ( 43.87500000054622973, 20.00000000000000355, 98.07665518445361386 ) ) ;
#1787 = DIRECTION ( 'NONE',  ( -1.000000000000000000, -0.000000000000000000, -0.000000000000000000 ) ) ;
#1788 = CARTESIAN_POINT ( 'NONE',  ( 5.000000000000000000, 50.00000000000000000, -24.49489742783178414 ) ) ;
#1789 = CARTESIAN_POINT ( 'NONE',  ( 48.09999999999998721, 17.56310227825320425, 98.29316153445363113 ) ) ;
#1790 = CARTESIAN_POINT ( 'NONE',  ( 41.69999999999998863, 26.37988106264029398, 95.42841645007781892 ) ) ;
#1791 = EDGE_CURVE ( 'NONE', #8970, #4148, #8893, .T. ) ;
#1792 = LINE ( 'NONE', #8464, #9290 ) ;
#1793 = VECTOR ( 'NONE', #6505, 1000.000000000000000 ) ;
#1794 = ORIENTED_EDGE ( 'NONE', *, *, #9260, .T. ) ;
#1795 = CARTESIAN_POINT ( 'NONE',  ( 35.95000000109247651, 13.62011893735971135, 95.42841645007781892 ) ) ;
#1796 = CARTESIAN_POINT ( 'NONE',  ( 24.89999999999998792, 17.56310227825320425, 83.29316153445363113 ) ) ;
#1797 = ORIENTED_EDGE ( 'NONE', *, *, #6355, .F. ) ;
#1798 = CARTESIAN_POINT ( 'NONE',  ( -27.49999999999999645, 20.00000000000000355, 170.0000119999999697 ) ) ;
#1799 = VERTEX_POINT ( 'NONE', #12340 ) ;
#1800 = CARTESIAN_POINT ( 'NONE',  ( -9.659227801817477754, 22.60918507870266581, -23.05884188866823337 ) ) ;
#1801 = EDGE_CURVE ( 'NONE', #3463, #5434, #2880, .T. ) ;
#1802 = DIRECTION ( 'NONE',  ( 1.000000000000000000, -0.000000000000000000, -0.000000000000000000 ) ) ;
#1803 =( GEOMETRIC_REPRESENTATION_CONTEXT ( 3 ) GLOBAL_UNCERTAINTY_ASSIGNED_CONTEXT ( ( #3906 ) ) GLOBAL_UNIT_ASSIGNED_CONTEXT ( ( #10776, #4188, #1465 ) ) REPRESENTATION_CONTEXT ( 'NONE', 'WORKASPACE' ) );
#1804 = CARTESIAN_POINT ( 'NONE',  ( -5.000000000000000888, 40.00000000000000000, 121.2488769092545198 ) ) ;
#1805 = AXIS2_PLACEMENT_3D ( 'NONE', #8515, #77, #7631 ) ;
#1806 = DIRECTION ( 'NONE',  ( 0.000000000000000000, 0.4999999999999983902, -0.8660254037844395958 ) ) ;
#1807 = CARTESIAN_POINT ( 'NONE',  ( 27.39999999999998792, 27.13292387221364876, 88.47553407664153724 ) ) ;
#1808 = EDGE_LOOP ( 'NONE', ( #6497, #12280, #6021, #8100, #4860, #11044 ) ) ;
#1809 = PLANE ( 'NONE',  #912 ) ;
#1810 = CARTESIAN_POINT ( 'NONE',  ( -4.147283247135973738, 10.89461892748662031, 27.69284716632408561 ) ) ;
#1811 = CARTESIAN_POINT ( 'NONE',  ( 20.17500000054622689, 13.07298590277314254, 93.04388485072563242 ) ) ;
#1812 = DIRECTION ( 'NONE',  ( 0.000000000000000000, 0.000000000000000000, 1.000000000000000000 ) ) ;
#1813 = DIRECTION ( 'NONE',  ( 0.000000000000000000, -0.5000000000000014433, -0.8660254037844379305 ) ) ;
#1814 = ORIENTED_EDGE ( 'NONE', *, *, #4472, .F. ) ;
#1815 = EDGE_LOOP ( 'NONE', ( #10593, #7293, #1188, #106 ) ) ;
#1816 = CARTESIAN_POINT ( 'NONE',  ( 21.69999999999998508, 26.37988106264029398, 95.42841645007781892 ) ) ;
#1817 = VECTOR ( 'NONE', #6496, 1000.000000000000000 ) ;
#1818 = DIRECTION ( 'NONE',  ( -0.000000000000000000, -0.000000000000000000, 1.000000000000000000 ) ) ;
#1819 = CARTESIAN_POINT ( 'NONE',  ( 20.17500000054622689, 13.07298590277314254, 93.04388485072563242 ) ) ;
#1820 = CARTESIAN_POINT ( 'NONE',  ( 6.000000000000000000, 6.760415694317218303E-15, 5.057500000000000995 ) ) ;
#1821 = FACE_OUTER_BOUND ( 'NONE', #2262, .T. ) ;
#1822 = CARTESIAN_POINT ( 'NONE',  ( -31.74999999999995737, 0.000000000000000000, 0.000000000000000000 ) ) ;
#1823 = CARTESIAN_POINT ( 'NONE',  ( 26.65000000109246514, 20.00000000000000355, 83.29316153445364534 ) ) ;
#1824 = CARTESIAN_POINT ( 'NONE',  ( 6.612460753110299017, 12.47060822435505756, 24.11434807139940517 ) ) ;
#1825 = ORIENTED_EDGE ( 'NONE', *, *, #1954, .T. ) ;
#1826 = VECTOR ( 'NONE', #9455, 1000.000000000000000 ) ;
#1827 = FACE_OUTER_BOUND ( 'NONE', #6135, .T. ) ;
#1828 = ADVANCED_FACE ( 'NONE', ( #3110 ), #8528, .F. ) ;
#1829 = DIRECTION ( 'NONE',  ( 0.000000000000000000, 0.000000000000000000, 1.000000000000000000 ) ) ;
#1830 = MANIFOLD_SOLID_BREP ( 'Hex', #2005 ) ;
#1831 = CARTESIAN_POINT ( 'NONE',  ( 28.87500000054622262, 20.00000000000000355, 83.50966788445364841 ) ) ;
#1832 = CARTESIAN_POINT ( 'NONE',  ( -2.000000000000015543, 20.00000000000000355, 98.29316153445363113 ) ) ;
#1833 = CARTESIAN_POINT ( 'NONE',  ( 40.87500000054622973, 22.36655054427230382, 83.50966788445364841 ) ) ;
#1834 = CARTESIAN_POINT ( 'NONE',  ( 28.17500000054621978, 13.80429023900056507, 95.29460816699764791 ) ) ;
#1835 = CARTESIAN_POINT ( 'NONE',  ( 26.59999999999998721, 12.86707612778636012, 88.47553407664152303 ) ) ;
#1836 = VECTOR ( 'NONE', #5214, 1000.000000000000114 ) ;
#1837 = CARTESIAN_POINT ( 'NONE',  ( 30.69999999999998863, 13.62011893735970958, 86.15790661882942914 ) ) ;
#1838 = CARTESIAN_POINT ( 'NONE',  ( 36.07500000054622546, 13.80429023900056507, 95.29460816699764791 ) ) ;
#1839 = EDGE_LOOP ( 'NONE', ( #11508, #2743, #7233, #12183, #8498, #2835, #829, #9052, #10546, #10410, #9366, #12012, #9085, #9441, #6536, #8348 ) ) ;
#1840 = CARTESIAN_POINT ( 'NONE',  ( 46.27500000054622120, 12.34168156654572535, 90.79316153445363113 ) ) ;
#1841 = CARTESIAN_POINT ( 'NONE',  ( 27.75000000109246301, 17.56310227825320425, 98.29316153445363113 ) ) ;
#1842 = EDGE_LOOP ( 'NONE', ( #6785, #12387, #10361, #9801 ) ) ;
#1843 = CARTESIAN_POINT ( 'NONE',  ( 7.513991638149614793, 13.39363280574569792, 19.61093064431749156 ) ) ;
#1844 = ORIENTED_EDGE ( 'NONE', *, *, #8243, .F. ) ;
#1845 = CARTESIAN_POINT ( 'NONE',  ( -2.000000000000015543, 20.00000000000000355, 83.29316153445364534 ) ) ;
#1846 = CARTESIAN_POINT ( 'NONE',  ( 32.59999999999998721, 12.86707612778636012, 88.47553407664152303 ) ) ;
#1847 = CARTESIAN_POINT ( 'NONE',  ( 0.000000000000000000, 0.000000000000000000, 0.000000000000000000 ) ) ;
#1848 = CARTESIAN_POINT ( 'NONE',  ( 46.97500000054621694, 22.36655054427230382, 83.50966788445364841 ) ) ;
#1849 = DIRECTION ( 'NONE',  ( 0.000000000000000000, 0.000000000000000000, -1.000000000000000000 ) ) ;
#1850 = EDGE_CURVE ( 'NONE', #9812, #2033, #12400, .T. ) ;
#1851 = FILL_AREA_STYLE_COLOUR ( '', #7188 ) ;
#1852 = CARTESIAN_POINT ( 'NONE',  ( 42.47500000054623115, 13.07298590277314432, 88.54243821818161564 ) ) ;
#1853 = CARTESIAN_POINT ( 'NONE',  ( 49.19999999999998863, 24.40838939219355197, 84.72553407664153724 ) ) ;
#1854 = CARTESIAN_POINT ( 'NONE',  ( 41.59999999999998721, 27.13292387221364876, 93.11078899226573924 ) ) ;
#1855 = DIRECTION ( 'NONE',  ( 0.000000000000000000, 0.000000000000000000, 1.000000000000000000 ) ) ;
#1856 = VERTEX_POINT ( 'NONE', #5970 ) ;
#1857 = EDGE_CURVE ( 'NONE', #5215, #5293, #312, .T. ) ;
#1858 = CARTESIAN_POINT ( 'NONE',  ( 36.05000000109246372, 12.86707612778636012, 93.11078899226572503 ) ) ;
#1859 = SURFACE_STYLE_FILL_AREA ( #6435 ) ;
#1860 = ORIENTED_EDGE ( 'NONE', *, *, #8899, .F. ) ;
#1861 = DIRECTION ( 'NONE',  ( 0.000000000000000000, 0.000000000000000000, -1.000000000000000000 ) ) ;
#1862 = ORIENTED_EDGE ( 'NONE', *, *, #475, .F. ) ;
#1863 = CARTESIAN_POINT ( 'NONE',  ( -5.845037936402837531, 28.12045204670673826, -24.30869324251348829 ) ) ;
#1864 = CARTESIAN_POINT ( 'NONE',  ( 3.061617454482527662E-15, 30.00000000000001066, 25.00000000000000000 ) ) ;
#1865 = CARTESIAN_POINT ( 'NONE',  ( -8.651571107376318182, 25.02565239439968536, 23.45586713013333124 ) ) ;
#1866 = CARTESIAN_POINT ( 'NONE',  ( 38.47500000054621694, 13.80429023900056684, 86.29171490190961435 ) ) ;
#1867 = DIRECTION ( 'NONE',  ( -1.000000000000000000, -0.000000000000000000, -0.000000000000000000 ) ) ;
#1868 = CARTESIAN_POINT ( 'NONE',  ( 4.999999999999999112, 0.000000000000000000, 169.9999999999999716 ) ) ;
#1869 = ORIENTED_EDGE ( 'NONE', *, *, #2322, .T. ) ;
#1870 = CARTESIAN_POINT ( 'NONE',  ( 3.973855183274129566, 53.05230689902806063, -27.71718999578467901 ) ) ;
#1871 = ADVANCED_FACE ( 'NONE', ( #4061 ), #5020, .T. ) ;
#1872 = CARTESIAN_POINT ( 'NONE',  ( -6.096819122263643642, 12.06690739318116812, 27.32937962794271414 ) ) ;
#1873 = CARTESIAN_POINT ( 'NONE',  ( 49.27500000054622120, 26.92701409722686634, 88.54243821818162985 ) ) ;
#1874 = ORIENTED_EDGE ( 'NONE', *, *, #2151, .T. ) ;
#1875 = CARTESIAN_POINT ( 'NONE',  ( -21.20617189303577987, 25.37779564132841159, 151.2938281069642130 ) ) ;
#1876 = DIRECTION ( 'NONE',  ( 0.000000000000000000, 0.000000000000000000, 1.000000000000000000 ) ) ;
#1877 = VERTEX_POINT ( 'NONE', #3700 ) ;
#1878 = VERTEX_POINT ( 'NONE', #7643 ) ;
#1879 = CIRCLE ( 'NONE', #6146, 9.000000000000000000 ) ;
#1880 = ADVANCED_FACE ( 'NONE', ( #8886, #203 ), #1675, .T. ) ;
#1881 = DIRECTION ( 'NONE',  ( 0.000000000000000000, 0.000000000000000000, -1.000000000000000000 ) ) ;
#1882 = B_SPLINE_CURVE_WITH_KNOTS ( 'NONE', 3,
 ( #5809, #11646, #9682, #9872, #166, #2055, #4985, #1185, #992, #7964, #293, #7899, #6939, #3963, #6062, #11832, #3139, #4155, #2191, #8030 ),
 .UNSPECIFIED., .F., .F.,
 ( 4, 2, 2, 2, 2, 2, 2, 2, 2, 4 ),
 ( 0.007833747489473694495, 0.008812489889827121448, 0.009791232290180546666, 0.01028060349035726101, 0.01076997469053397535, 0.01174871709088740057, 0.01272745949124082926, 0.01370620189159425448, 0.01468494429194768143, 0.01566368669230110838 ),
 .UNSPECIFIED. ) ;
#1883 = CYLINDRICAL_SURFACE ( 'NONE', #1171, 28.00000000000000355 ) ;
#1884 = CARTESIAN_POINT ( 'NONE',  ( 21.07500000054622546, 26.19570976099943849, 86.29171490190961435 ) ) ;
#1885 = CARTESIAN_POINT ( 'NONE',  ( 9.960637755725160858, 18.97835903059869622, 98.24092394347138679 ) ) ;
#1886 = CARTESIAN_POINT ( 'NONE',  ( 6.000000000000000000, 0.000000000000000000, 0.000000000000000000 ) ) ;
#1887 = CARTESIAN_POINT ( 'NONE',  ( 3.765166081389465624, 46.69397311189987931, -20.66103212045354098 ) ) ;
#1888 = CARTESIAN_POINT ( 'NONE',  ( 10.00000000000000355, 20.00000000000000355, 106.9999999999999574 ) ) ;
#1889 = CARTESIAN_POINT ( 'NONE',  ( -31.74999999999995737, 1.102182119232617714E-15, -9.000000000000000000 ) ) ;
#1890 = ORIENTED_EDGE ( 'NONE', *, *, #7052, .F. ) ;
#1891 = CARTESIAN_POINT ( 'NONE',  ( 37.55000000109244951, 22.43689772174683128, 98.29316153445361692 ) ) ;
#1892 = VECTOR ( 'NONE', #5489, 999.9999999999998863 ) ;
#1893 = AXIS2_PLACEMENT_3D ( 'NONE', #4279, #7320, #8219 ) ;
#1894 = CARTESIAN_POINT ( 'NONE',  ( 24.25000000109246301, 12.86707612778636012, 88.47553407664152303 ) ) ;
#1895 = CARTESIAN_POINT ( 'NONE',  ( 38.67500000054623399, 17.63344945572770328, 83.50966788445364841 ) ) ;
#1896 = CARTESIAN_POINT ( 'NONE',  ( 26.47500000054622404, 13.07298590277314432, 88.54243821818161564 ) ) ;
#1897 = CARTESIAN_POINT ( 'NONE',  ( 31.29999999999998650, 26.37988106264029398, 86.15790661882942914 ) ) ;
#1898 = ADVANCED_FACE ( 'NONE', ( #3762 ), #5558, .F. ) ;
#1899 = CARTESIAN_POINT ( 'NONE',  ( 30.37500000054622973, 13.07298590277314432, 88.54243821818161564 ) ) ;
#1900 = ORIENTED_EDGE ( 'NONE', *, *, #11408, .T. ) ;
#1901 = CYLINDRICAL_SURFACE ( 'NONE', #10138, 6.000000000000003553 ) ;
#1902 = ORIENTED_EDGE ( 'NONE', *, *, #9179, .T. ) ;
#1903 = CARTESIAN_POINT ( 'NONE',  ( 6.000000000000000000, -4.379923479639793449, 2.528750000000004494 ) ) ;
#1904 = ORIENTED_EDGE ( 'NONE', *, *, #9414, .T. ) ;
#1905 =( NAMED_UNIT ( * ) SI_UNIT ( $, .STERADIAN. ) SOLID_ANGLE_UNIT ( ) );
#1906 = CARTESIAN_POINT ( 'NONE',  ( 27.50000000000000355, 27.49999999999999645, 145.0000000000000000 ) ) ;
#1907 = CARTESIAN_POINT ( 'NONE',  ( 9.983665987661890284, 19.33903170736681432, -26.15965704797978830 ) ) ;
#1908 = CARTESIAN_POINT ( 'NONE',  ( 45.37500000054622973, 27.65831843345427998, 90.79316153445363113 ) ) ;
#1909 = CARTESIAN_POINT ( 'NONE',  ( 6.000000000000000000, 5.839897972853064445, -8.673617379884035472E-15 ) ) ;
#1910 = CARTESIAN_POINT ( 'NONE',  ( -50.00000000000001421, 69.50000000000000000, 101.8533255156881978 ) ) ;
#1911 = CARTESIAN_POINT ( 'NONE',  ( 47.17500000054622689, 26.19570976099943493, 86.29171490190961435 ) ) ;
#1912 = CARTESIAN_POINT ( 'NONE',  ( 21.17500000054622689, 26.19570976099943493, 86.29171490190961435 ) ) ;
#1913 = CARTESIAN_POINT ( 'NONE',  ( 45.09999999999998721, 22.43689772174682417, 83.29316153445364534 ) ) ;
#1914 = ADVANCED_FACE ( 'NONE', ( #9428 ), #3148, .F. ) ;
#1915 = DIRECTION ( 'NONE',  ( -0.000000000000000000, -0.000000000000000000, 1.000000000000000000 ) ) ;
#1916 = EDGE_LOOP ( 'NONE', ( #1063, #4190, #6240, #9780 ) ) ;
#1917 = CARTESIAN_POINT ( 'NONE',  ( 31.35000000109246088, 26.37988106264029398, 95.42841645007781892 ) ) ;
#1918 = CARTESIAN_POINT ( 'NONE',  ( 2.610381677634093123, 10.34108370468245219, 24.86537221636008965 ) ) ;
#1919 = ORIENTED_EDGE ( 'NONE', *, *, #7603, .T. ) ;
#1920 = ADVANCED_FACE ( 'NONE', ( #2694, #4787 ), #12523, .T. ) ;
#1921 = ORIENTED_EDGE ( 'NONE', *, *, #10279, .T. ) ;
#1922 = LINE ( 'NONE', #4852, #1017 ) ;
#1923 = PRODUCT_DEFINITION_SHAPE ( 'NONE', 'NONE',  #9616 ) ;
#1924 = TOROIDAL_SURFACE ( 'NONE', #8612, 6.500000000000000888, 1.500000000000000000 ) ;
#1925 = CARTESIAN_POINT ( 'NONE',  ( -50.00000000000001421, 40.00000000000000000, 132.8533255156884820 ) ) ;
#1926 = DIRECTION ( 'NONE',  ( 0.000000000000000000, 0.000000000000000000, -1.000000000000000000 ) ) ;
#1927 = CARTESIAN_POINT ( 'NONE',  ( 36.57500000054622546, 15.71886984736413773, 84.90069139318163138 ) ) ;
#1928 = VECTOR ( 'NONE', #3092, 1000.000000000000000 ) ;
#1929 = CARTESIAN_POINT ( 'NONE',  ( 10.00000000000000355, 20.00000000000000355, 22.91287847477919826 ) ) ;
#1930 = CARTESIAN_POINT ( 'NONE',  ( 44.65000000109246514, 20.00000000000000355, 83.29316153445364534 ) ) ;
#1931 = CARTESIAN_POINT ( 'NONE',  ( 33.85000000109246798, 15.59161060780645691, 96.86078899226572503 ) ) ;
#1932 = VERTEX_POINT ( 'NONE', #5056 ) ;
#1933 = CARTESIAN_POINT ( 'NONE',  ( 10.00000000000000355, 20.00000000000000355, 26.15339366124404563 ) ) ;
#1934 = LINE ( 'NONE', #6508, #6749 ) ;
#1935 = CARTESIAN_POINT ( 'NONE',  ( 21.37500000054622618, 26.92701409722686634, 93.04388485072563242 ) ) ;
#1936 = VERTEX_POINT ( 'NONE', #7844 ) ;
#1937 = CARTESIAN_POINT ( 'NONE',  ( 46.05000000109246372, 12.86707612778636012, 93.11078899226572503 ) ) ;
#1938 = EDGE_CURVE ( 'NONE', #1672, #3699, #10627, .T. ) ;
#1939 = EDGE_CURVE ( 'NONE', #10127, #9490, #8790, .T. ) ;
#1940 = CARTESIAN_POINT ( 'NONE',  ( 4.492685090163540451, 52.21864068105092116, -20.51419621738226695 ) ) ;
#1941 = EDGE_LOOP ( 'NONE', ( #7827, #5400, #1312, #11371 ) ) ;
#1942 = VERTEX_POINT ( 'NONE', #171 ) ;
#1943 = CARTESIAN_POINT ( 'NONE',  ( 21.59999999999998721, 27.13292387221364876, 93.11078899226573924 ) ) ;
#1944 = EDGE_CURVE ( 'NONE', #8208, #113, #237, .T. ) ;
#1945 = CARTESIAN_POINT ( 'NONE',  ( 0.000000000000000000, 0.000000000000000000, 0.000000000000000000 ) ) ;
#1946 = DIRECTION ( 'NONE',  ( 0.000000000000000000, 0.000000000000000000, 1.000000000000000000 ) ) ;
#1947 = CARTESIAN_POINT ( 'NONE',  ( 4.839602763736350788, 48.70207075804894714, -24.52717836283222752 ) ) ;
#1948 = CARTESIAN_POINT ( 'NONE',  ( -0.3317315395883421170, 55.00000000000000711, -21.00000000000000000 ) ) ;
#1949 = DIRECTION ( 'NONE',  ( 0.000000000000000000, -0.000000000000000000, 1.000000000000000000 ) ) ;
#1950 = AXIS2_PLACEMENT_3D ( 'NONE', #5127, #9946, #7914 ) ;
#1952 = EDGE_CURVE ( 'NONE', #9442, #5929, #11048, .T. ) ;
#1951 =( BOUNDED_CURVE ( )  B_SPLINE_CURVE ( 2, ( #2547, #7560, #8332, #6660, #9348, #10529, #897, #1719, #10343, #1841, #9590 ),
 .UNSPECIFIED., .F., .F. ) 
 B_SPLINE_CURVE_WITH_KNOTS ( ( 3, 2, 2, 2, 2, 3 ),
 ( 0.6999999999999999556, 0.7066666666666666652, 0.7133333333333333748, 0.7199999999999999734, 0.7266666666666666829, 0.7333333333333332815 ),
 .UNSPECIFIED. ) 
 CURVE ( )  GEOMETRIC_REPRESENTATION_ITEM ( )  RATIONAL_B_SPLINE_CURVE ( ( 1.000000000000000000, 0.9510565162951535312, 1.000000000000000000, 0.9510565162951535312, 1.000000000000000000, 0.9510565162951535312, 1.000000000000000000, 0.9510565162951535312, 1.000000000000000000, 0.9510565162951535312, 1.000000000000000000 ) ) 
 REPRESENTATION_ITEM ( '' )  );
#1953 = CARTESIAN_POINT ( 'NONE',  ( 1.613533685434110465, 45.25622145510568828, 27.95510990066616941 ) ) ;
#1954 = EDGE_CURVE ( 'NONE', #938, #637, #2198, .T. ) ;
#1955 = DIRECTION ( 'NONE',  ( 1.000000000000000000, 0.000000000000000000, 0.000000000000000000 ) ) ;
#1956 = ORIENTED_EDGE ( 'NONE', *, *, #11423, .F. ) ;
#1957 = CARTESIAN_POINT ( 'NONE',  ( 0.000000000000000000, 0.000000000000000000, 0.000000000000000000 ) ) ;
#1958 = COLOUR_RGB ( '',0.7921568627450980005, 0.8196078431372548767, 0.9333333333333333481 ) ;
#1959 = DIRECTION ( 'NONE',  ( -1.000000000000000000, -0.000000000000000000, -0.000000000000000000 ) ) ;
#1960 = CARTESIAN_POINT ( 'NONE',  ( 39.57500000054622546, 24.28113015263587116, 96.68563167572563088 ) ) ;
#1961 = CARTESIAN_POINT ( 'NONE',  ( 28.97500000054622404, 22.36655054427230382, 83.50966788445364841 ) ) ;
#1962 = CARTESIAN_POINT ( 'NONE',  ( 25.59999999999998721, 27.13292387221364876, 93.11078899226573924 ) ) ;
#1963 = CARTESIAN_POINT ( 'NONE',  ( 34.19999999999998863, 15.59161060780645691, 96.86078899226572503 ) ) ;
#1964 = CARTESIAN_POINT ( 'NONE',  ( 34.97500000054623115, 24.28113015263587471, 84.90069139318163138 ) ) ;
#1965 = ORIENTED_EDGE ( 'NONE', *, *, #9329, .T. ) ;
#1966 = CARTESIAN_POINT ( 'NONE',  ( 1.500000000000001332, 9.797174393178825657E-16, -8.000000000000000000 ) ) ;
#1967 = AXIS2_PLACEMENT_3D ( 'NONE', #3895, #3202, #1114 ) ;
#1968 = ORIENTED_EDGE ( 'NONE', *, *, #8089, .T. ) ;
#1969 = CARTESIAN_POINT ( 'NONE',  ( 3.429011071898990822E-15, 55.00000000000000000, 28.00000000000000355 ) ) ;
#1970 = EDGE_LOOP ( 'NONE', ( #8362, #11591, #8204 ) ) ;
#1971 = CARTESIAN_POINT ( 'NONE',  ( -50.00000000000001421, 77.00000000000000000, 94.35332551568819781 ) ) ;
#1972 = CARTESIAN_POINT ( 'NONE',  ( 47.57500000054621836, 26.19570976099943849, 95.29460816699764791 ) ) ;
#1973 = DIRECTION ( 'NONE',  ( 0.000000000000000000, 1.000000000000000000, 0.000000000000000000 ) ) ;
#1974 = DIRECTION ( 'NONE',  ( 0.000000000000000000, 0.000000000000000000, -1.000000000000000000 ) ) ;
#1975 = CARTESIAN_POINT ( 'NONE',  ( 44.47500000054622404, 13.07298590277314432, 88.54243821818161564 ) ) ;
#1976 = CARTESIAN_POINT ( 'NONE',  ( 39.69999999999997442, 26.37988106264029398, 95.42841645007781892 ) ) ;
#1977 = CARTESIAN_POINT ( 'NONE',  ( 40.49999999999998579, 12.11403331821300533, 90.79316153445363113 ) ) ;
#1978 = LINE ( 'NONE', #9732, #5852 ) ;
#1979 = VERTEX_POINT ( 'NONE', #4863 ) ;
#1980 = CARTESIAN_POINT ( 'NONE',  ( 33.95000000109246940, 13.62011893735971135, 95.42841645007781892 ) ) ;
#1981 = FACE_BOUND ( 'NONE', #10869, .T. ) ;
#1982 = EDGE_LOOP ( 'NONE', ( #9506, #9877, #7134, #2757, #7198 ) ) ;
#1983 = VECTOR ( 'NONE', #10062, 1000.000000000000000 ) ;
#1984 = ORIENTED_EDGE ( 'NONE', *, *, #1388, .T. ) ;
#1985 = CARTESIAN_POINT ( 'NONE',  ( -34.72841614740048044, 22.00000000000000000, 152.2284161474004520 ) ) ;
#1986 = CARTESIAN_POINT ( 'NONE',  ( -5.000000000000000000, 50.00000000000000000, -24.49489742783178059 ) ) ;
#1987 = ADVANCED_FACE ( 'NONE', ( #4925, #3903 ), #6823, .T. ) ;
#1988 = CARTESIAN_POINT ( 'NONE',  ( 0.000000000000000000, 139.9999999999999716, -25.00000000000000000 ) ) ;
#1989 = AXIS2_PLACEMENT_3D ( 'NONE', #5639, #4746, #9512 ) ;
#1990 = CARTESIAN_POINT ( 'NONE',  ( 33.87500000054621552, 17.63344945572769973, 98.07665518445361386 ) ) ;
#1991 = CARTESIAN_POINT ( 'NONE',  ( 40.67500000054622689, 15.71886984736413773, 84.90069139318163138 ) ) ;
#1992 = CARTESIAN_POINT ( 'NONE',  ( 34.75000000109243814, 22.43689772174679575, 83.29316153445363113 ) ) ;
#1993 = CARTESIAN_POINT ( 'NONE',  ( -10.00000000000000355, 20.00000000000000355, 18.46618531261938756 ) ) ;
#1994 = CARTESIAN_POINT ( 'NONE',  ( -2.000000000000015543, 20.00000000000000355, 90.79316153445363113 ) ) ;
#1995 = PRESENTATION_LAYER_ASSIGNMENT (  '', '', ( #5855 ) ) ;
#1996 = VERTEX_POINT ( 'NONE', #1998 ) ;
#1997 = CARTESIAN_POINT ( 'NONE',  ( 48.65000000109246514, 20.00000000000000355, 83.29316153445364534 ) ) ;
#1998 = CARTESIAN_POINT ( 'NONE',  ( 28.99999999999998934, 20.00000000000000355, 83.29316153445364534 ) ) ;
#1999 = ORIENTED_EDGE ( 'NONE', *, *, #6207, .F. ) ;
#2000 = DIRECTION ( 'NONE',  ( -1.000000000000000000, -0.000000000000000000, -0.000000000000000000 ) ) ;
#2001 = UNCERTAINTY_MEASURE_WITH_UNIT (LENGTH_MEASURE( 1.000000000000000082E-05 ), #12461, 'distance_accuracy_value', 'NONE');
#2002 = ORIENTED_EDGE ( 'NONE', *, *, #1262, .F. ) ;
#2003 = TOROIDAL_SURFACE ( 'NONE', #3824, 13.85889894354065355, 10.00000000000000000 ) ;
#2004 = VERTEX_POINT ( 'NONE', #5878 ) ;
#2005 = CLOSED_SHELL ( 'NONE', ( #2536, #9645, #12084, #12329, #9249, #8671, #1321, #5617, #4519, #10116, #1987, #7678, #1113, #5280, #6311, #3115, #1871, #5075, #4886, #10073, #4577, #2570, #9477, #3656, #3912, #4181, #11801 ) ) ;
#2006 = CARTESIAN_POINT ( 'NONE',  ( 21.49999999999998934, 27.88596668178699645, 90.79316153445363113 ) ) ;
#2007 = CARTESIAN_POINT ( 'NONE',  ( 0.000000000000000000, 0.000000000000000000, 0.000000000000000000 ) ) ;
#2008 = EDGE_CURVE ( 'NONE', #11777, #5465, #109, .T. ) ;
#2009 = CARTESIAN_POINT ( 'NONE',  ( 9.919782953541179893, 21.28887143972310625, 83.40037394667403703 ) ) ;
#2010 = DIRECTION ( 'NONE',  ( -1.000000000000000000, -0.000000000000000000, -0.000000000000000000 ) ) ;
#2011 = CARTESIAN_POINT ( 'NONE',  ( 1.653699482248477182, 29.86790856825577478, 20.93734097219926582 ) ) ;
#2012 = CARTESIAN_POINT ( 'NONE',  ( 32.00000000000000000, 0.000000000000000000, 0.000000000000000000 ) ) ;
#2013 = CARTESIAN_POINT ( 'NONE',  ( 3.048292328532992368, 46.02321945503342704, 27.83491629969137904 ) ) ;
#2014 = CARTESIAN_POINT ( 'NONE',  ( 92.00000000000000000, 0.000000000000000000, 0.000000000000000000 ) ) ;
#2015 = ORIENTED_EDGE ( 'NONE', *, *, #9935, .F. ) ;
#2016 = DIRECTION ( 'NONE',  ( -1.000000000000000000, -0.000000000000000000, -0.000000000000000000 ) ) ;
#2017 = AXIS2_PLACEMENT_3D ( 'NONE', #2923, #8885, #8819 ) ;
#2018 = EDGE_CURVE ( 'NONE', #7797, #1292, #5646, .T. ) ;
#2019 = CARTESIAN_POINT ( 'NONE',  ( 24.17500000054622333, 13.80429023900056507, 95.29460816699764791 ) ) ;
#2020 = CARTESIAN_POINT ( 'NONE',  ( 49.77500000054621410, 22.36655054427230027, 98.07665518445361386 ) ) ;
#2021 = CARTESIAN_POINT ( 'NONE',  ( 34.07500000054622546, 13.80429023900056507, 95.29460816699764791 ) ) ;
#2022 =( BOUNDED_CURVE ( )  B_SPLINE_CURVE ( 3, ( #2325, #111, #11776, #3970 ),
 .UNSPECIFIED., .F., .F. ) 
 B_SPLINE_CURVE_WITH_KNOTS ( ( 4, 4 ),
 ( 4.712388980384689674, 6.283185307179585344 ),
 .UNSPECIFIED. ) 
 CURVE ( )  GEOMETRIC_REPRESENTATION_ITEM ( )  RATIONAL_B_SPLINE_CURVE ( ( 1.000000000000000000, 0.8047378541243649375, 0.8047378541243649375, 1.000000000000000000 ) ) 
 REPRESENTATION_ITEM ( '' )  );
#2023 = CARTESIAN_POINT ( 'NONE',  ( -1.002883791299520887E-19, 10.00000000000000000, -25.00000000000000000 ) ) ;
#2024 = CARTESIAN_POINT ( 'NONE',  ( 25.39999999999998792, 27.13292387221364876, 88.47553407664153724 ) ) ;
#2025 = CARTESIAN_POINT ( 'NONE',  ( 49.49999999999997868, 27.88596668178699645, 90.79316153445363113 ) ) ;
#2026 = CARTESIAN_POINT ( 'NONE',  ( 30.87500000054622618, 22.36655054427230382, 83.50966788445364841 ) ) ;
#2027 = ORIENTED_EDGE ( 'NONE', *, *, #456, .F. ) ;
#2028 = CIRCLE ( 'NONE', #12370, 25.00000000000000000 ) ;
#2029 = ADVANCED_FACE ( 'NONE', ( #11256 ), #3275, .F. ) ;
#2030 = DIRECTION ( 'NONE',  ( -0.000000000000000000, -0.000000000000000000, -1.000000000000000000 ) ) ;
#2031 = VERTEX_POINT ( 'NONE', #10186 ) ;
#2032 = CARTESIAN_POINT ( 'NONE',  ( 48.95000000109246940, 26.37988106264029398, 86.15790661882942914 ) ) ;
#2033 = VERTEX_POINT ( 'NONE', #8347 ) ;
#2034 = CARTESIAN_POINT ( 'NONE',  ( 5.000000000000000000, 50.00000000000000000, -24.49489742783178414 ) ) ;
#2035 = CARTESIAN_POINT ( 'NONE',  ( -2.000000000000015543, 20.00000000000000355, 98.29316153445363113 ) ) ;
#2036 = EDGE_CURVE ( 'NONE', #11366, #9971, #3393, .T. ) ;
#2037 = CARTESIAN_POINT ( 'NONE',  ( 37.27500000054622831, 26.92701409722686634, 88.54243821818162985 ) ) ;
#2038 = DIRECTION ( 'NONE',  ( 0.000000000000000000, 0.000000000000000000, 1.000000000000000000 ) ) ;
#2039 = CARTESIAN_POINT ( 'NONE',  ( -34.72841614740047333, 18.00000000000000355, 152.2284161474004520 ) ) ;
#2040 = CARTESIAN_POINT ( 'NONE',  ( 37.47500000054622404, 26.92701409722686634, 93.04388485072563242 ) ) ;
#2041 = CARTESIAN_POINT ( 'NONE',  ( 39.79999999999999005, 24.40838939219354842, 96.86078899226572503 ) ) ;
#2042 = CARTESIAN_POINT ( 'NONE',  ( 40.19999999999998863, 15.59161060780645691, 96.86078899226572503 ) ) ;
#2043 = DIRECTION ( 'NONE',  ( 0.000000000000000000, -0.4999999999999983902, 0.8660254037844395958 ) ) ;
#2044 = VERTEX_POINT ( 'NONE', #5183 ) ;
#2045 = CARTESIAN_POINT ( 'NONE',  ( 29.05000000109246727, 27.13292387221364876, 88.47553407664153724 ) ) ;
#2046 = LINE ( 'NONE', #2111, #12359 ) ;
#2047 = ORIENTED_EDGE ( 'NONE', *, *, #94, .F. ) ;
#2048 = AXIS2_PLACEMENT_3D ( 'NONE', #1588, #9578, #11357 ) ;
#2049 = EDGE_LOOP ( 'NONE', ( #5398, #4959, #5054, #8702, #10093 ) ) ;
#2050 = CARTESIAN_POINT ( 'NONE',  ( -9.355575343945487177, 23.54668771876638189, -23.18385937405269459 ) ) ;
#2051 = DIRECTION ( 'NONE',  ( 0.000000000000000000, 0.000000000000000000, 1.000000000000000000 ) ) ;
#2052 = CARTESIAN_POINT ( 'NONE',  ( 0.6000000000000033085, 0.000000000000000000, 0.000000000000000000 ) ) ;
#2053 = CARTESIAN_POINT ( 'NONE',  ( 35.97500000054623115, 15.71886984736413417, 96.68563167572563088 ) ) ;
#2054 = CARTESIAN_POINT ( 'NONE',  ( 31.97500000054622760, 17.63344945572769973, 98.07665518445361386 ) ) ;
#2055 = CARTESIAN_POINT ( 'NONE',  ( -2.066793275460399926, 54.55579475875813245, 27.92402955534884512 ) ) ;
#2056 = CARTESIAN_POINT ( 'NONE',  ( 9.357332009350985302, 23.54206009522648202, -26.39048829257603401 ) ) ;
#2057 = DIRECTION ( 'NONE',  ( 1.000000000000000000, 0.000000000000000000, 0.000000000000000000 ) ) ;
#2058 = ORIENTED_EDGE ( 'NONE', *, *, #7609, .F. ) ;
#2059 = CARTESIAN_POINT ( 'NONE',  ( 49.47500000054623115, 26.92701409722686634, 93.04388485072563242 ) ) ;
#2060 = DIRECTION ( 'NONE',  ( -1.000000000000000000, -0.000000000000000000, -0.000000000000000000 ) ) ;
#2061 = ORIENTED_EDGE ( 'NONE', *, *, #4367, .F. ) ;
#2062 = EDGE_CURVE ( 'NONE', #1674, #9622, #12153, .T. ) ;
#2063 = FACE_OUTER_BOUND ( 'NONE', #8114, .T. ) ;
#2064 = MANIFOLD_SOLID_BREP ( 'Chamfer1', #11527 ) ;
#2065 = ORIENTED_EDGE ( 'NONE', *, *, #5531, .T. ) ;
#2066 = ORIENTED_EDGE ( 'NONE', *, *, #319, .F. ) ;
#2067 = CARTESIAN_POINT ( 'NONE',  ( 121.9999999999999858, 6.167321280506070407E-16, -5.035999999999999588 ) ) ;
#2068 = CARTESIAN_POINT ( 'NONE',  ( -31.00470515163596019, 27.49999999999999645, 148.5047051516359318 ) ) ;
#2069 = CARTESIAN_POINT ( 'NONE',  ( 7.928408809296215054, 26.09658529048988740, 95.16773376593604894 ) ) ;
#2070 = CARTESIAN_POINT ( 'NONE',  ( 43.99999999999999289, 20.00000000000000355, 98.29316153445363113 ) ) ;
#2071 = DIRECTION ( 'NONE',  ( 1.000000000000000000, -0.000000000000000000, -0.000000000000000000 ) ) ;
#2072 = LINE ( 'NONE', #5003, #10396 ) ;
#2073 = CARTESIAN_POINT ( 'NONE',  ( 2.636325768737970421, 29.66875067697592883, -20.84397515108148724 ) ) ;
#2074 = CARTESIAN_POINT ( 'NONE',  ( 41.17500000054623399, 26.92701409722686634, 88.54243821818162985 ) ) ;
#2075 = AXIS2_PLACEMENT_3D ( 'NONE', #4841, #8707, #9787 ) ;
#2076 = DIRECTION ( 'NONE',  ( 0.000000000000000000, -1.000000000000000000, 1.039664082171044875E-15 ) ) ;
#2077 = ORIENTED_EDGE ( 'NONE', *, *, #5139, .T. ) ;
#2078 = CARTESIAN_POINT ( 'NONE',  ( 10.00000000000000355, 20.00000000000000355, -22.91287847477919826 ) ) ;
#2079 = EDGE_CURVE ( 'NONE', #9848, #8345, #9051, .T. ) ;
#2080 = APPLICATION_PROTOCOL_DEFINITION ( 'draft international standard', 'automotive_design', 1998, #7150 ) ;
#2081 = MANIFOLD_SOLID_BREP ( 'Fillet1', #9111 ) ;
#2082 = PRODUCT_RELATED_PRODUCT_CATEGORY ( 'part', '', ( #6099 ) ) ;
#2083 = DIRECTION ( 'NONE',  ( 0.000000000000000000, 1.000000000000000000, -1.336710962791342904E-15 ) ) ;
#2084 = CARTESIAN_POINT ( 'NONE',  ( 48.27500000054622831, 13.07298590277314254, 93.04388485072563242 ) ) ;
#2085 = EDGE_CURVE ( 'NONE', #850, #4258, #4664, .T. ) ;
#2086 = CARTESIAN_POINT ( 'NONE',  ( 35.17500000054622689, 26.92701409722686634, 88.54243821818162985 ) ) ;
#2087 = CARTESIAN_POINT ( 'NONE',  ( 20.47500000054622404, 13.07298590277314432, 88.54243821818161564 ) ) ;
#2088 = CARTESIAN_POINT ( 'NONE',  ( 24.99999999999998579, 20.00000000000000355, 83.29316153445364534 ) ) ;
#2089 = CARTESIAN_POINT ( 'NONE',  ( 49.79999999999999005, 24.40838939219354842, 96.86078899226572503 ) ) ;
#2090 = CARTESIAN_POINT ( 'NONE',  ( 30.47500000054622404, 13.80429023900056684, 86.29171490190961435 ) ) ;
#2091 = ORIENTED_EDGE ( 'NONE', *, *, #6451, .T. ) ;
#2092 = DIRECTION ( 'NONE',  ( 0.000000000000000000, 0.000000000000000000, 1.000000000000000000 ) ) ;
#2093 = DIRECTION ( 'NONE',  ( -0.000000000000000000, -0.000000000000000000, 1.000000000000000000 ) ) ;
#2094 = ORIENTED_EDGE ( 'NONE', *, *, #9469, .F. ) ;
#2095 = CARTESIAN_POINT ( 'NONE',  ( 10.00000000000000178, 9.797174393178825657E-16, -8.000000000000000000 ) ) ;
#2096 = ORIENTED_EDGE ( 'NONE', *, *, #11173, .T. ) ;
#2097 = DIRECTION ( 'NONE',  ( -1.000000000000000000, -0.000000000000000000, -0.000000000000000000 ) ) ;
#2098 = DIRECTION ( 'NONE',  ( 1.000000000000000000, 0.000000000000000000, 0.000000000000000000 ) ) ;
#2099 = CARTESIAN_POINT ( 'NONE',  ( 40.27500000054622120, 13.07298590277314254, 93.04388485072563242 ) ) ;
#2100 = CARTESIAN_POINT ( 'NONE',  ( 6.000000000000000000, -2.919948986426538440, -5.057499999999997442 ) ) ;
#2101 = EDGE_CURVE ( 'NONE', #9553, #5036, #11989, .T. ) ;
#2102 = CARTESIAN_POINT ( 'NONE',  ( 49.67500000054621978, 22.36655054427230027, 98.07665518445361386 ) ) ;
#2103 = CARTESIAN_POINT ( 'NONE',  ( 41.17500000054621978, 26.19570976099943493, 86.29171490190961435 ) ) ;
#2104 = CARTESIAN_POINT ( 'NONE',  ( 44.09999999999998010, 17.56310227825320425, 98.29316153445363113 ) ) ;
#2105 = VECTOR ( 'NONE', #12328, 1000.000000000000000 ) ;
#2106 = CARTESIAN_POINT ( 'NONE',  ( -10.00000000000000533, 20.66054119461773553, -22.91287847477919470 ) ) ;
#2107 = CARTESIAN_POINT ( 'NONE',  ( 13.64110105645934290, 20.00000000000000355, 197.9999999999999716 ) ) ;
#2108 = VERTEX_POINT ( 'NONE', #8589 ) ;
#2109 = AXIS2_PLACEMENT_3D ( 'NONE', #447, #4560, #11286 ) ;
#2110 = CARTESIAN_POINT ( 'NONE',  ( 29.35000000109245732, 26.37988106264029398, 95.42841645007781892 ) ) ;
#2111 = CARTESIAN_POINT ( 'NONE',  ( 6.000000000000000000, -2.919948986426523341, 5.057500000000002771 ) ) ;
#2112 = EDGE_LOOP ( 'NONE', ( #1527, #7808, #11520, #1542 ) ) ;
#2113 = EDGE_CURVE ( 'NONE', #8906, #11777, #788, .T. ) ;
#2114 = EDGE_CURVE ( 'NONE', #6763, #2160, #5850, .T. ) ;
#2115 = ORIENTED_EDGE ( 'NONE', *, *, #908, .T. ) ;
#2116 = CARTESIAN_POINT ( 'NONE',  ( 9.661529737047111155, 17.39944252900632193, 26.28051061400176991 ) ) ;
#2117 = CARTESIAN_POINT ( 'NONE',  ( -4.493909509445460415, 52.21603442804438799, -24.59310644668742540 ) ) ;
#2118 = AXIS2_PLACEMENT_3D ( 'NONE', #11844, #5419, #9289 ) ;
#2119 = CARTESIAN_POINT ( 'NONE',  ( -50.00000000000001421, 0.000000000000000000, 69.99999999999998579 ) ) ;
#2120 = CARTESIAN_POINT ( 'NONE',  ( 28.77500000054622831, 20.00000000000000355, 83.50966788445364841 ) ) ;
#2121 = CARTESIAN_POINT ( 'NONE',  ( 32.57500000054621836, 13.80429023900056684, 86.29171490190961435 ) ) ;
#2122 = CARTESIAN_POINT ( 'NONE',  ( 44.25000000109246656, 12.86707612778636012, 88.47553407664152303 ) ) ;
#2123 = CARTESIAN_POINT ( 'NONE',  ( 0.000000000000000000, 2.919948986426526005, -5.057500000000003659 ) ) ;
#2124 = EDGE_LOOP ( 'NONE', ( #4978, #8968, #10794, #2582, #3424, #204, #9766, #4611, #9474, #963, #4270, #1676, #233, #7725, #1265, #2770 ) ) ;
#2125 = CARTESIAN_POINT ( 'NONE',  ( 49.37500000054622262, 27.65831843345427998, 90.79316153445363113 ) ) ;
#2126 = CARTESIAN_POINT ( 'NONE',  ( 2.221110608488543026, 54.49139573732541209, -24.90296241992962578 ) ) ;
#2127 = DIRECTION ( 'NONE',  ( 1.000000000000000000, 0.000000000000000000, 0.000000000000000000 ) ) ;
#2128 = EDGE_LOOP ( 'NONE', ( #5597, #9875 ) ) ;
#2129 = DIRECTION ( 'NONE',  ( 0.000000000000000000, 0.000000000000000000, 1.000000000000000000 ) ) ;
#2130 = AXIS2_PLACEMENT_3D ( 'NONE', #11454, #2761, #2825 ) ;
#2131 = ORIENTED_EDGE ( 'NONE', *, *, #6444, .T. ) ;
#2132 = DIRECTION ( 'NONE',  ( 0.000000000000000000, -1.000000000000000000, 1.110768649713241713E-15 ) ) ;
#2133 = CARTESIAN_POINT ( 'NONE',  ( -1.643512924178977430, 10.13039013404520716, -24.94805769307042453 ) ) ;
#2134 = DIRECTION ( 'NONE',  ( -0.000000000000000000, 1.000000000000000000, 1.224646799147353207E-16 ) ) ;
#2135 = CARTESIAN_POINT ( 'NONE',  ( 27.49999999999999645, 20.00000000000000355, 170.0000119999999697 ) ) ;
#2136 = PRODUCT_DEFINITION_SHAPE ( 'NONE', 'NONE',  #240 ) ;
#2137 = AXIS2_PLACEMENT_3D ( 'NONE', #4802, #2768, #3905 ) ;
#2138 = FACE_OUTER_BOUND ( 'NONE', #12282, .T. ) ;
#2139 = DIRECTION ( 'NONE',  ( 1.000000000000000000, -0.000000000000000000, -0.000000000000000000 ) ) ;
#2140 = CARTESIAN_POINT ( 'NONE',  ( 9.931121997304011018, 21.34393702597181530, 18.50391133509319630 ) ) ;
#2141 = CARTESIAN_POINT ( 'NONE',  ( -1.614845647245295668, 54.74348708565381827, 20.94004496404980742 ) ) ;
#2142 = LINE ( 'NONE', #1261, #9038 ) ;
#2143 = CARTESIAN_POINT ( 'NONE',  ( 44.07500000054623968, 13.80429023900056507, 95.29460816699764791 ) ) ;
#2144 = CIRCLE ( 'NONE', #6394, 5.035999999999999588 ) ;
#2145 = CARTESIAN_POINT ( 'NONE',  ( 4.999999999999999112, 49.66826422043975242, 20.39607805437114507 ) ) ;
#2146 = ORIENTED_EDGE ( 'NONE', *, *, #2414, .F. ) ;
#2147 = CARTESIAN_POINT ( 'NONE',  ( 9.104442389086463194, 24.14915179589751304, -23.28362858151144721 ) ) ;
#2148 = PRODUCT_CONTEXT ( 'NONE', #9350, 'mechanical' ) ;
#2149 =( BOUNDED_CURVE ( )  B_SPLINE_CURVE ( 3, ( #6892, #8992, #3913, #10631 ),
 .UNSPECIFIED., .F., .F. ) 
 B_SPLINE_CURVE_WITH_KNOTS ( ( 4, 4 ),
 ( 3.141592653589793560, 4.712388980384689674 ),
 .UNSPECIFIED. ) 
 CURVE ( )  GEOMETRIC_REPRESENTATION_ITEM ( )  RATIONAL_B_SPLINE_CURVE ( ( 1.000000000000000000, 0.8047378541243650485, 0.8047378541243650485, 1.000000000000000000 ) ) 
 REPRESENTATION_ITEM ( '' )  );
#2150 = MANIFOLD_SOLID_BREP ( 'Cut-Extrude1[1]', #9310 ) ;
#2151 = EDGE_CURVE ( 'NONE', #1332, #8919, #2692, .T. ) ;
#2152 = CARTESIAN_POINT ( 'NONE',  ( 20.67500000054622689, 15.71886984736413773, 84.90069139318163138 ) ) ;
#2153 = CARTESIAN_POINT ( 'NONE',  ( 24.35000000109246798, 13.62011893735970958, 86.15790661882942914 ) ) ;
#2154 = CONICAL_SURFACE ( 'NONE', #142, 6.999999999999978684, 0.7853981633974473908 ) ;
#2155 = CARTESIAN_POINT ( 'NONE',  ( 34.37500000054622973, 13.07298590277314432, 88.54243821818161564 ) ) ;
#2156 = CARTESIAN_POINT ( 'NONE',  ( 21.77500000054622831, 22.36655054427230027, 98.07665518445361386 ) ) ;
#2157 = CARTESIAN_POINT ( 'NONE',  ( 26.09999999999998721, 17.56310227825320425, 98.29316153445363113 ) ) ;
#2158 = CARTESIAN_POINT ( 'NONE',  ( 5.000000000000000000, 4.685197434473814759, -5.637851296924623057E-15 ) ) ;
#2159 = CARTESIAN_POINT ( 'NONE',  ( 29.17500000054623044, 26.92701409722686634, 88.54243821818162985 ) ) ;
#2160 = VERTEX_POINT ( 'NONE', #4596 ) ;
#2161 = FACE_OUTER_BOUND ( 'NONE', #5184, .T. ) ;
#2162 = ORIENTED_EDGE ( 'NONE', *, *, #4585, .F. ) ;
#2163 = CARTESIAN_POINT ( 'NONE',  ( 4.871799307858193373, 51.13674912335573453, 27.57293273687329105 ) ) ;
#2164 = ORIENTED_EDGE ( 'NONE', *, *, #6150, .T. ) ;
#2165 = CIRCLE ( 'NONE', #11477, 0.4000000000000001887 ) ;
#2166 = CARTESIAN_POINT ( 'NONE',  ( -3.973726775714538029, 53.05247132632594287, -24.68286527305685141 ) ) ;
#2167 = DIRECTION ( 'NONE',  ( -0.000000000000000000, -0.000000000000000000, 1.000000000000000000 ) ) ;
#2168 = CARTESIAN_POINT ( 'NONE',  ( 37.57500000054622546, 26.19570976099943849, 95.29460816699764791 ) ) ;
#2169 = DIRECTION ( 'NONE',  ( 0.000000000000000000, -0.000000000000000000, 1.000000000000000000 ) ) ;
#2170 = CARTESIAN_POINT ( 'NONE',  ( 26.09999999999998366, 17.56310227825320425, 98.29316153445363113 ) ) ;
#2171 = CARTESIAN_POINT ( 'NONE',  ( 40.97500000054622404, 22.36655054427230382, 83.50966788445364841 ) ) ;
#2172 = CARTESIAN_POINT ( 'NONE',  ( 39.99999999999998579, 20.00000000000000355, 98.29316153445363113 ) ) ;
#2173 = EDGE_CURVE ( 'NONE', #3634, #9164, #1778, .T. ) ;
#2174 = EDGE_CURVE ( 'NONE', #5616, #409, #4144, .T. ) ;
#2175 = DIRECTION ( 'NONE',  ( -1.000000000000000000, 0.000000000000000000, 0.000000000000000000 ) ) ;
#2176 = CARTESIAN_POINT ( 'NONE',  ( -10.00000000000000355, 20.00000000000000355, -28.00000000000000711 ) ) ;
#2177 = VERTEX_POINT ( 'NONE', #10734 ) ;
#2178 = CARTESIAN_POINT ( 'NONE',  ( 31.15000000109245804, 27.88596668178699645, 90.79316153445363113 ) ) ;
#2179 = CARTESIAN_POINT ( 'NONE',  ( 40.65000000109246514, 20.00000000000000355, 83.29316153445364534 ) ) ;
#2180 = EDGE_LOOP ( 'NONE', ( #6946, #7322, #9894, #5335, #11443, #10716 ) ) ;
#2181 = CARTESIAN_POINT ( 'NONE',  ( 0.6582936873354101603, 54.96735637312282563, -20.99215814668205482 ) ) ;
#2182 = EDGE_LOOP ( 'NONE', ( #7575, #1902, #6930, #1965, #2594 ) ) ;
#2183 = CARTESIAN_POINT ( 'NONE',  ( 3.545294789778632882, 10.64386042719674919, 27.77630898643412394 ) ) ;
#2184 = VECTOR ( 'NONE', #1785, 1000.000000000000000 ) ;
#2185 = DIRECTION ( 'NONE',  ( 0.000000000000000000, 0.000000000000000000, 1.000000000000000000 ) ) ;
#2186 = LINE ( 'NONE', #1988, #5156 ) ;
#2187 = PRODUCT_DEFINITION_CONTEXT ( 'detailed design', #7150, 'design' ) ;
#2188 = EDGE_CURVE ( 'NONE', #10800, #6113, #7, .T. ) ;
#2189 = CARTESIAN_POINT ( 'NONE',  ( 30.57500000054622902, 15.71886984736413773, 84.90069139318163138 ) ) ;
#2190 = CARTESIAN_POINT ( 'NONE',  ( 29.97500000054622404, 17.63344945572769973, 98.07665518445361386 ) ) ;
#2191 = CARTESIAN_POINT ( 'NONE',  ( -5.000000000000000888, 50.32659431431049057, 27.54995462791181993 ) ) ;
#2192 = CARTESIAN_POINT ( 'NONE',  ( 90.00000000000000000, 4.171999999999999709, 0.000000000000000000 ) ) ;
#2193 = DIRECTION ( 'NONE',  ( -1.000000000000000000, -0.000000000000000000, -0.000000000000000000 ) ) ;
#2194 = AXIS2_PLACEMENT_3D ( 'NONE', #6493, #9485, #5678 ) ;
#2195 = ORIENTED_EDGE ( 'NONE', *, *, #4213, .T. ) ;
#2196 = CARTESIAN_POINT ( 'NONE',  ( 48.07500000054622546, 15.71886984736413417, 96.68563167572563088 ) ) ;
#2197 = CARTESIAN_POINT ( 'NONE',  ( 48.25000000109246656, 12.86707612778636012, 88.47553407664152303 ) ) ;
#2198 = LINE ( 'NONE', #7074, #12270 ) ;
#2199 = ORIENTED_EDGE ( 'NONE', *, *, #11568, .F. ) ;
#2200 = DIRECTION ( 'NONE',  ( 0.000000000000000000, -0.000000000000000000, 1.000000000000000000 ) ) ;
#2201 = EDGE_CURVE ( 'NONE', #2752, #10467, #5726, .T. ) ;
#2202 = VERTEX_POINT ( 'NONE', #3889 ) ;
#2203 = CARTESIAN_POINT ( 'NONE',  ( -31.00470515163596019, 12.50000000000001066, 148.5047051516359318 ) ) ;
#2204 = CARTESIAN_POINT ( 'NONE',  ( -9.461967865576259129, 16.74741879838144598, -18.74787822604630350 ) ) ;
#2205 = EDGE_CURVE ( 'NONE', #4253, #7687, #2046, .T. ) ;
#2206 = CIRCLE ( 'NONE', #10910, 8.000000000000000000 ) ;
#2207 = CARTESIAN_POINT ( 'NONE',  ( 49.77500000054622831, 20.00000000000000355, 98.07665518445361386 ) ) ;
#2208 = CARTESIAN_POINT ( 'NONE',  ( 27.49999999999999645, 20.00000000000000355, 171.0000000000000000 ) ) ;
#2209 = CARTESIAN_POINT ( 'NONE',  ( 9.241050560303825989, 23.84658578115114480, 97.24969729302414123 ) ) ;
#2210 = PLANE ( 'NONE',  #577 ) ;
#2211 = CARTESIAN_POINT ( 'NONE',  ( 10.00000000000000355, 20.00000000000000355, 18.46618531261938401 ) ) ;
#2212 = CARTESIAN_POINT ( 'NONE',  ( -2.222896043811084077, 54.49078271291326558, 20.88425106962813516 ) ) ;
#2213 = DIRECTION ( 'NONE',  ( 0.000000000000000000, 1.224646799147351728E-16, 1.000000000000000000 ) ) ;
#2214 = CIRCLE ( 'NONE', #4035, 10.00000000000000355 ) ;
#2215 = APPLICATION_CONTEXT ( 'automotive_design' ) ;
#2216 = CARTESIAN_POINT ( 'NONE',  ( 41.67500000054622689, 22.36655054427230027, 98.07665518445361386 ) ) ;
#2217 = CARTESIAN_POINT ( 'NONE',  ( 3.304159235005521111, 46.23328646880356274, 20.73974243245384841 ) ) ;
#2218 = ORIENTED_EDGE ( 'NONE', *, *, #4435, .F. ) ;
#2219 = DIRECTION ( 'NONE',  ( 0.7071067811865469066, 8.659560562354926695E-17, -0.7071067811865482389 ) ) ;
#2220 = CONICAL_SURFACE ( 'NONE', #3510, 4.171999999999999709, 0.7853981633974609355 ) ;
#2221 = B_SPLINE_CURVE_WITH_KNOTS ( 'NONE', 3,
 ( #2549, #7310, #2486, #10173, #9037, #2426, #2308, #9163, #591, #12200, #8086, #11241, #4331, #531, #5230, #8334, #3446, #6304, #3500, #6177, #4392, #350, #7184, #10053, #4271, #1364 ),
 .UNSPECIFIED., .F., .F.,
 ( 4, 2, 2, 2, 2, 2, 2, 2, 2, 2, 2, 2, 4 ),
 ( 0.01576777909941014244, 0.01675267178542435773, 0.01773756447143857301, 0.01970734984346701052, 0.02167713521549544456, 0.02266202790150966331, 0.02364692058752388554, 0.02561670595955232305, 0.02660159864556654180, 0.02758649133158076056, 0.02955627670360919113, 0.03054116938962340988, 0.03152606207563762863 ),
 .UNSPECIFIED. ) ;
#2222 = CARTESIAN_POINT ( 'NONE',  ( 20.77500000054622120, 17.63344945572770328, 83.50966788445364841 ) ) ;
#2223 = CARTESIAN_POINT ( 'NONE',  ( 47.37500000054622973, 27.65831843345427998, 90.79316153445363113 ) ) ;
#2224 = CARTESIAN_POINT ( 'NONE',  ( 34.67500000054621268, 17.63344945572770328, 83.50966788445364841 ) ) ;
#2225 = VECTOR ( 'NONE', #4273, 1000.000000000000000 ) ;
#2226 = CARTESIAN_POINT ( 'NONE',  ( 20.87500000054622262, 20.00000000000000355, 83.50966788445364841 ) ) ;
#2227 = CARTESIAN_POINT ( 'NONE',  ( 25.99999999999998934, 20.00000000000000355, 98.29316153445363113 ) ) ;
#2228 = SURFACE_STYLE_FILL_AREA ( #6096 ) ;
#2229 = CARTESIAN_POINT ( 'NONE',  ( 28.27500000054622475, 12.34168156654572535, 90.79316153445363113 ) ) ;
#2230 = ORIENTED_EDGE ( 'NONE', *, *, #11650, .F. ) ;
#2231 = EDGE_CURVE ( 'NONE', #1292, #2612, #7764, .T. ) ;
#2232 = DIRECTION ( 'NONE',  ( -1.000000000000000000, -0.000000000000000000, -0.000000000000000000 ) ) ;
#2233 = ORIENTED_EDGE ( 'NONE', *, *, #8936, .T. ) ;
#2234 = ORIENTED_EDGE ( 'NONE', *, *, #3811, .T. ) ;
#2235 = EDGE_CURVE ( 'NONE', #7100, #3380, #7707, .T. ) ;
#2236 = PLANE ( 'NONE',  #9151 ) ;
#2237 = ORIENTED_EDGE ( 'NONE', *, *, #7463, .T. ) ;
#2238 = PLANE ( 'NONE',  #7415 ) ;
#2239 = CARTESIAN_POINT ( 'NONE',  ( 39.37500000054622262, 27.65831843345427998, 90.79316153445363113 ) ) ;
#2240 = DIRECTION ( 'NONE',  ( 1.000000000000000000, -0.000000000000000000, -0.000000000000000000 ) ) ;
#2241 = DIRECTION ( 'NONE',  ( 1.000000000000000000, -0.000000000000000000, -0.000000000000000000 ) ) ;
#2242 = CARTESIAN_POINT ( 'NONE',  ( 38.37500000054622973, 12.34168156654572535, 90.79316153445363113 ) ) ;
#2243 = CARTESIAN_POINT ( 'NONE',  ( 41.79999999999999005, 24.40838939219354842, 96.86078899226572503 ) ) ;
#2244 = VECTOR ( 'NONE', #2740, 1000.000000000000000 ) ;
#2245 = CARTESIAN_POINT ( 'NONE',  ( 47.07500000054622546, 26.19570976099943493, 86.29171490190961435 ) ) ;
#2246 = ORIENTED_EDGE ( 'NONE', *, *, #9611, .T. ) ;
#2247 = CARTESIAN_POINT ( 'NONE',  ( 23.55000000109246017, 22.43689772174679575, 98.29316153445363113 ) ) ;
#2248 = CARTESIAN_POINT ( 'NONE',  ( -3.304393266822325703, 46.23318141187127139, 24.78176792680001839 ) ) ;
#2249 = VERTEX_POINT ( 'NONE', #2179 ) ;
#2250 = DIRECTION ( 'NONE',  ( -1.000000000000000000, 0.000000000000000000, -0.000000000000000000 ) ) ;
#2251 = VERTEX_POINT ( 'NONE', #10605 ) ;
#2252 = CIRCLE ( 'NONE', #4058, 7.499999999999992895 ) ;
#2253 = DIRECTION ( 'NONE',  ( 0.000000000000000000, 0.000000000000000000, -1.000000000000000000 ) ) ;
#2254 = PRODUCT_DEFINITION_SHAPE ( 'NONE', 'NONE',  #12547 ) ;
#2255 = ADVANCED_FACE ( 'NONE', ( #1981, #4013 ), #5038, .F. ) ;
#2256 = CARTESIAN_POINT ( 'NONE',  ( 27.47500000054622404, 26.19570976099943493, 95.29460816699764791 ) ) ;
#2257 = CARTESIAN_POINT ( 'NONE',  ( 33.77500000054623541, 22.36655054427230027, 98.07665518445361386 ) ) ;
#2258 = EDGE_CURVE ( 'NONE', #1279, #2352, #4503, .T. ) ;
#2259 = PLANE ( 'NONE',  #4747 ) ;
#2260 = CARTESIAN_POINT ( 'NONE',  ( -5.000000000000000888, 0.000000000000000000, 169.9999999999999716 ) ) ;
#2261 = CARTESIAN_POINT ( 'NONE',  ( 37.65000000109246514, 20.00000000000000355, 98.29316153445363113 ) ) ;
#2262 = EDGE_LOOP ( 'NONE', ( #5500, #669, #9036, #8194 ) ) ;
#2263 = AXIS2_PLACEMENT_3D ( 'NONE', #7059, #11461, #2250 ) ;
#2264 = CARTESIAN_POINT ( 'NONE',  ( 46.55000000109245661, 17.56310227825321135, 83.29316153445363113 ) ) ;
#2265 = VERTEX_POINT ( 'NONE', #3376 ) ;
#2266 = CARTESIAN_POINT ( 'NONE',  ( -32.89339828220179385, 84.49999999999998579, 151.2467237978899846 ) ) ;
#2267 = ORIENTED_EDGE ( 'NONE', *, *, #2996, .T. ) ;
#2268 = CARTESIAN_POINT ( 'NONE',  ( -3.251483927478052482, 10.53766038749295753, -20.74918120701668300 ) ) ;
#2269 = DIRECTION ( 'NONE',  ( 0.000000000000000000, -1.224646799147353207E-16, 1.000000000000000000 ) ) ;
#2270 = CARTESIAN_POINT ( 'NONE',  ( 4.491430111798321967, 52.22103771687890372, 24.59356092490497758 ) ) ;
#2271 = EDGE_CURVE ( 'NONE', #5152, #7013, #6332, .T. ) ;
#2272 = CARTESIAN_POINT ( 'NONE',  ( 9.842430534136942910, 21.78601360974349532, 83.50449544991025164 ) ) ;
#2273 = CARTESIAN_POINT ( 'NONE',  ( 22.99999999999998934, 20.00000000000000355, 83.29316153445364534 ) ) ;
#2274 = CARTESIAN_POINT ( 'NONE',  ( -2.509809017951089682, 45.66333224303983229, -24.87518608377025231 ) ) ;
#2275 = CARTESIAN_POINT ( 'NONE',  ( -0.3310653830415872800, 54.99172937625127133, 20.99802641299722339 ) ) ;
#2276 = DIRECTION ( 'NONE',  ( 1.000000000000000000, 0.000000000000000000, 0.000000000000000000 ) ) ;
#2277 = CARTESIAN_POINT ( 'NONE',  ( 42.07500000054623257, 13.80429023900056507, 95.29460816699764791 ) ) ;
#2278 = CARTESIAN_POINT ( 'NONE',  ( -4.484481976314367735, 47.78274414339135490, -24.59462526944309246 ) ) ;
#2279 = VERTEX_POINT ( 'NONE', #10934 ) ;
#2280 = EDGE_CURVE ( 'NONE', #7452, #724, #11754, .T. ) ;
#2281 = CARTESIAN_POINT ( 'NONE',  ( -1.614380680224908104, 54.74360302825979119, 24.94967786989446878 ) ) ;
#2282 = CARTESIAN_POINT ( 'NONE',  ( 46.89999999999999858, 17.56310227825318648, 83.29316153445365956 ) ) ;
#2283 = CARTESIAN_POINT ( 'NONE',  ( 46.17500000054622689, 13.80429023900056507, 95.29460816699764791 ) ) ;
#2284 = CARTESIAN_POINT ( 'NONE',  ( 30.97500000054622760, 24.28113015263587471, 84.90069139318163138 ) ) ;
#2285 = CARTESIAN_POINT ( 'NONE',  ( 21.87500000054622618, 20.00000000000000355, 98.07665518445361386 ) ) ;
#2286 = LINE ( 'NONE', #11993, #4845 ) ;
#2287 = CARTESIAN_POINT ( 'NONE',  ( 28.47500000054622404, 13.80429023900056684, 86.29171490190961435 ) ) ;
#2288 = ORIENTED_EDGE ( 'NONE', *, *, #7234, .T. ) ;
#2289 = CARTESIAN_POINT ( 'NONE',  ( -19.99999999999999645, 20.00000000000000355, 170.0000119999999697 ) ) ;
#2290 = EDGE_LOOP ( 'NONE', ( #1544, #10095, #11839, #11489 ) ) ;
#2291 = ORIENTED_EDGE ( 'NONE', *, *, #11576, .T. ) ;
#2292 = CARTESIAN_POINT ( 'NONE',  ( 38.10000000000000142, 17.56310227825315451, 98.29316153445357429 ) ) ;
#2293 = ORIENTED_EDGE ( 'NONE', *, *, #6989, .F. ) ;
#2294 =( LENGTH_UNIT ( ) NAMED_UNIT ( * ) SI_UNIT ( .MILLI., .METRE. ) );
#2295 = AXIS2_PLACEMENT_3D ( 'NONE', #6970, #7929, #130 ) ;
#2296 = CARTESIAN_POINT ( 'NONE',  ( 36.67500000054622689, 15.71886984736413773, 84.90069139318163138 ) ) ;
#2297 = PLANE ( 'NONE',  #12015 ) ;
#2298 = EDGE_CURVE ( 'NONE', #8987, #2922, #11550, .T. ) ;
#2299 = CARTESIAN_POINT ( 'NONE',  ( -5.000000000000000000, 50.00000000000000000, -27.54995462791182703 ) ) ;
#2300 = CARTESIAN_POINT ( 'NONE',  ( 42.37500000054621552, 12.34168156654572535, 90.79316153445363113 ) ) ;
#2301 = CARTESIAN_POINT ( 'NONE',  ( 37.19999999999998863, 24.40838939219355197, 84.72553407664153724 ) ) ;
#2302 = CARTESIAN_POINT ( 'NONE',  ( 47.67500000054622689, 22.36655054427230027, 98.07665518445361386 ) ) ;
#2303 = EDGE_LOOP ( 'NONE', ( #8019, #1900, #4267, #4455 ) ) ;
#2304 = AXIS2_PLACEMENT_3D ( 'NONE', #620, #1507, #12167 ) ;
#2305 = CARTESIAN_POINT ( 'NONE',  ( 22.25000000109246656, 12.86707612778636012, 88.47553407664152303 ) ) ;
#2306 = CARTESIAN_POINT ( 'NONE',  ( -5.000000000000000000, 50.00000000000000000, 24.49489742783178414 ) ) ;
#2307 = VERTEX_POINT ( 'NONE', #406 ) ;
#2308 = CARTESIAN_POINT ( 'NONE',  ( -3.240369384686552223, 29.48342856360252640, 27.81866359660341814 ) ) ;
#2309 = ORIENTED_EDGE ( 'NONE', *, *, #7493, .F. ) ;
#2310 = CARTESIAN_POINT ( 'NONE',  ( 24.75000000109246301, 22.43689772174679575, 83.29316153445363113 ) ) ;
#2311 = CARTESIAN_POINT ( 'NONE',  ( 40.85000000109246088, 24.40838939219355197, 84.72553407664153724 ) ) ;
#2312 = DIRECTION ( 'NONE',  ( 0.000000000000000000, 0.000000000000000000, -1.000000000000000000 ) ) ;
#2313 = TOROIDAL_SURFACE ( 'NONE', #4129, 8.400000000000000355, 0.5999999999999999778 ) ;
#2314 = EDGE_CURVE ( 'NONE', #5337, #3004, #588, .T. ) ;
#2315 = CARTESIAN_POINT ( 'NONE',  ( 29.97500000054622760, 15.71886984736413417, 96.68563167572563088 ) ) ;
#2316 = CARTESIAN_POINT ( 'NONE',  ( 31.77500000054622475, 22.36655054427230027, 98.07665518445361386 ) ) ;
#2317 = CIRCLE ( 'NONE', #501, 6.000000000000000000 ) ;
#2318 = B_SPLINE_CURVE_WITH_KNOTS ( 'NONE', 3,
 ( #11987, #4369, #3415, #7284, #2459, #6335, #10202, #9324, #8364, #1514, #8306, #12174, #3477, #7409, #6151, #2525, #5455, #10026, #8118, #6515 ),
 .UNSPECIFIED., .F., .F.,
 ( 4, 2, 2, 2, 2, 2, 2, 2, 2, 4 ),
 ( 0.02350813035260379893, 0.02448705762280033518, 0.02546598489299686796, 0.02644491216319340421, 0.02693437579829167233, 0.02742383943338994046, 0.02840276670358647670, 0.02938169397378300948, 0.03036062124397954226, 0.03133954851417607851 ),
 .UNSPECIFIED. ) ;
#2319 = CARTESIAN_POINT ( 'NONE',  ( 6.110050479722892725, 27.94346550729981971, 27.33088603378091008 ) ) ;
#2320 = CARTESIAN_POINT ( 'NONE',  ( 6.000000000000000000, 2.919948986426538884, 5.057499999999996554 ) ) ;
#2321 = ORIENTED_EDGE ( 'NONE', *, *, #8532, .F. ) ;
#2322 = EDGE_CURVE ( 'NONE', #8906, #5150, #11889, .T. ) ;
#2323 = CARTESIAN_POINT ( 'NONE',  ( 44.85000000109246798, 24.40838939219355197, 84.72553407664153724 ) ) ;
#2324 = VERTEX_POINT ( 'NONE', #4329 ) ;
#2325 = CARTESIAN_POINT ( 'NONE',  ( 27.50000000000000355, 12.50000000000001066, 145.0000000000000000 ) ) ;
#2326 = ORIENTED_EDGE ( 'NONE', *, *, #175, .F. ) ;
#2327 = VECTOR ( 'NONE', #6640, 1000.000000000000000 ) ;
#2328 = CARTESIAN_POINT ( 'NONE',  ( 10.00000000000000355, 20.00000000000000355, -66.99999999999998579 ) ) ;
#2329 = CARTESIAN_POINT ( 'NONE',  ( -7.519134213638725583, 26.60056234660722652, 23.84343405217310874 ) ) ;
#2330 = CARTESIAN_POINT ( 'NONE',  ( 20.17500000054622689, 13.07298590277314254, 93.04388485072563242 ) ) ;
#2331 = DIRECTION ( 'NONE',  ( 0.000000000000000000, -0.7071067811865479058, -0.7071067811865471286 ) ) ;
#2332 = CARTESIAN_POINT ( 'NONE',  ( 31.99999999999998579, 20.00000000000000355, 98.29316153445363113 ) ) ;
#2333 = DIRECTION ( 'NONE',  ( -0.000000000000000000, -0.000000000000000000, 1.000000000000000000 ) ) ;
#2334 = EDGE_CURVE ( 'NONE', #3380, #2943, #7056, .T. ) ;
#2335 = CARTESIAN_POINT ( 'NONE',  ( -10.00000000000000355, 19.33860219128660063, 18.46618531261938045 ) ) ;
#2336 = CARTESIAN_POINT ( 'NONE',  ( 90.00000000000000000, 0.000000000000000000, 0.000000000000000000 ) ) ;
#2337 = CARTESIAN_POINT ( 'NONE',  ( -0.3303383338888909448, 45.00000000000002132, 28.00000000000001066 ) ) ;
#2338 = CARTESIAN_POINT ( 'NONE',  ( 2.506524500420500345, 45.66117316082983990, 20.85169879525578907 ) ) ;
#2339 = EDGE_LOOP ( 'NONE', ( #10440, #5022, #6178, #7639 ) ) ;
#2340 = PLANE ( 'NONE',  #1392 ) ;
#2341 = EDGE_CURVE ( 'NONE', #6176, #6723, #3452, .T. ) ;
#2342 = CONTEXT_DEPENDENT_SHAPE_REPRESENTATION ( #11525, #328 ) ;
#2343 = CARTESIAN_POINT ( 'NONE',  ( 0.6000000000000033085, 1.102182119232617714E-15, -9.000000000000000000 ) ) ;
#2344 = CARTESIAN_POINT ( 'NONE',  ( 46.67500000054622689, 15.71886984736413773, 84.90069139318163138 ) ) ;
#2345 = CARTESIAN_POINT ( 'NONE',  ( 25.57500000054622546, 24.28113015263587116, 96.68563167572563088 ) ) ;
#2346 = EDGE_CURVE ( 'NONE', #10081, #1979, #2366, .T. ) ;
#2347 = CARTESIAN_POINT ( 'NONE',  ( 9.844713702461632465, 18.22664983694489749, 83.50141417594349491 ) ) ;
#2348 = CARTESIAN_POINT ( 'NONE',  ( 44.85000000109246798, 24.40838939219355197, 84.72553407664153724 ) ) ;
#2349 = AXIS2_PLACEMENT_3D ( 'NONE', #5446, #4485, #10688 ) ;
#2350 = CARTESIAN_POINT ( 'NONE',  ( 30.99999999999998934, 20.00000000000000355, 83.29316153445364534 ) ) ;
#2351 = CARTESIAN_POINT ( 'NONE',  ( 27.07500000054622902, 26.19570976099943493, 86.29171490190961435 ) ) ;
#2352 = VERTEX_POINT ( 'NONE', #4269 ) ;
#2353 = FACE_OUTER_BOUND ( 'NONE', #11122, .T. ) ;
#2354 = VERTEX_POINT ( 'NONE', #8145 ) ;
#2355 = CARTESIAN_POINT ( 'NONE',  ( 37.99999999999999289, 20.00000000000000355, 98.29316153445363113 ) ) ;
#2356 = ORIENTED_EDGE ( 'NONE', *, *, #8239, .T. ) ;
#2357 = SHAPE_REPRESENTATION_RELATIONSHIP ( 'NONE' , 'NONE' ,  #3370, #8540 ) ;
#2358 = CARTESIAN_POINT ( 'NONE',  ( 31.27500000054622831, 26.92701409722686634, 88.54243821818162985 ) ) ;
#2359 = CARTESIAN_POINT ( 'NONE',  ( 0.000000000000000000, 1.065442715258197248E-15, -8.400000000000000355 ) ) ;
#2360 = CARTESIAN_POINT ( 'NONE',  ( 20.15000000109246514, 12.11403331821300533, 90.79316153445363113 ) ) ;
#2361 = CARTESIAN_POINT ( 'NONE',  ( 34.87500000054622262, 20.00000000000000355, 83.50966788445364841 ) ) ;
#2362 = CARTESIAN_POINT ( 'NONE',  ( 35.50000000000000000, 27.88596668178699645, 90.79316153445363113 ) ) ;
#2363 = CARTESIAN_POINT ( 'NONE',  ( 46.27500000054622120, 12.34168156654572535, 90.79316153445363113 ) ) ;
#2364 = VERTEX_POINT ( 'NONE', #3618 ) ;
#2365 = CARTESIAN_POINT ( 'NONE',  ( 27.85000000109246443, 15.59161060780645691, 96.86078899226572503 ) ) ;
#2366 = LINE ( 'NONE', #466, #3850 ) ;
#2367 = VECTOR ( 'NONE', #2399, 1000.000000000000000 ) ;
#2368 = ORIENTED_EDGE ( 'NONE', *, *, #10302, .T. ) ;
#2369 =( BOUNDED_CURVE ( )  B_SPLINE_CURVE ( 2, ( #9596, #3748, #10594, #903, #1846, #8639, #4773, #2930, #4899, #10536, #2867 ),
 .UNSPECIFIED., .F., .F. ) 
 B_SPLINE_CURVE_WITH_KNOTS ( ( 3, 2, 2, 2, 2, 3 ),
 ( 0.5666666666666666519, 0.5733333333333333615, 0.5799999999999999600, 0.5866666666666666696, 0.5933333333333333792, 0.5999999999999999778 ),
 .UNSPECIFIED. ) 
 CURVE ( )  GEOMETRIC_REPRESENTATION_ITEM ( )  RATIONAL_B_SPLINE_CURVE ( ( 1.000000000000000000, 0.9510565162951535312, 1.000000000000000000, 0.9510565162951535312, 1.000000000000000000, 0.9510565162951535312, 1.000000000000000000, 0.9510565162951535312, 1.000000000000000000, 0.9510565162951535312, 1.000000000000000000 ) ) 
 REPRESENTATION_ITEM ( '' )  );
#2370 = CARTESIAN_POINT ( 'NONE',  ( 18.00000000000000355, 20.00000000000000355, 171.0000000000000000 ) ) ;
#2371 = ORIENTED_EDGE ( 'NONE', *, *, #4079, .F. ) ;
#2372 = DIRECTION ( 'NONE',  ( 1.000000000000000000, 0.000000000000000000, 0.000000000000000000 ) ) ;
#2373 = CARTESIAN_POINT ( 'NONE',  ( 27.49999999999999645, 20.00000000000000355, 187.9999999999999716 ) ) ;
#2374 = DIRECTION ( 'NONE',  ( 0.000000000000000000, 0.000000000000000000, -1.000000000000000000 ) ) ;
#2375 = CARTESIAN_POINT ( 'NONE',  ( 33.37500000054622973, 26.92701409722686634, 93.04388485072563242 ) ) ;
#2376 = CARTESIAN_POINT ( 'NONE',  ( 27.77500000054622475, 22.36655054427230027, 98.07665518445361386 ) ) ;
#2377 = DIRECTION ( 'NONE',  ( 0.000000000000000000, 1.000000000000000000, -1.336710962791342904E-15 ) ) ;
#2378 = ORIENTED_EDGE ( 'NONE', *, *, #9357, .T. ) ;
#2379 = CARTESIAN_POINT ( 'NONE',  ( 43.75000000109246656, 17.56310227825320425, 98.29316153445363113 ) ) ;
#2380 = CARTESIAN_POINT ( 'NONE',  ( 6.000000000000000000, 6.193651186687738874E-16, -5.057500000000000107 ) ) ;
#2381 = EDGE_LOOP ( 'NONE', ( #5658, #1440, #5927, #9300, #2834 ) ) ;
#2382 = DIRECTION ( 'NONE',  ( 1.000000000000000000, -0.000000000000000000, 0.000000000000000000 ) ) ;
#2383 = ORIENTED_EDGE ( 'NONE', *, *, #7457, .F. ) ;
#2384 = EDGE_CURVE ( 'NONE', #2615, #3714, #711, .T. ) ;
#2385 = CARTESIAN_POINT ( 'NONE',  ( -4.451684831872904091, 11.03962932791216112, -20.52483624935579343 ) ) ;
#2386 = CARTESIAN_POINT ( 'NONE',  ( -5.303430480311382311, 28.48399989248413178, 24.43255084236253794 ) ) ;
#2387 = FILL_AREA_STYLE_COLOUR ( '', #750 ) ;
#2388 = CARTESIAN_POINT ( 'NONE',  ( -10.00000000000000355, 20.00000000000000355, 22.91287847477919826 ) ) ;
#2389 = CARTESIAN_POINT ( 'NONE',  ( 6.000000000000000000, 5.839897972853065333, -6.938893903907228378E-15 ) ) ;
#2390 = DIRECTION ( 'NONE',  ( 0.000000000000000000, 0.000000000000000000, -1.000000000000000000 ) ) ;
#2391 = CARTESIAN_POINT ( 'NONE',  ( -9.483022228547349997, 16.75970615777680450, 26.34659568642391392 ) ) ;
#2392 = DIRECTION ( 'NONE',  ( 1.000000000000000000, -0.000000000000000000, -0.000000000000000000 ) ) ;
#2393 = EDGE_LOOP ( 'NONE', ( #2964, #2456, #5123, #3875, #4597 ) ) ;
#2394 = VECTOR ( 'NONE', #9999, 1000.000000000000000 ) ;
#2395 = CARTESIAN_POINT ( 'NONE',  ( -9.674976284561235929, 17.38768585986672122, -26.27572687994997835 ) ) ;
#2396 = MECHANICAL_DESIGN_GEOMETRIC_PRESENTATION_REPRESENTATION (  '', ( #6254 ), #7120 ) ;
#2397 = CARTESIAN_POINT ( 'NONE',  ( 0.3271393060908659445, 45.00000000000000711, 25.00000000000000355 ) ) ;
#2398 = EDGE_CURVE ( 'NONE', #11698, #2695, #4652, .T. ) ;
#2399 = DIRECTION ( 'NONE',  ( 0.000000000000000000, 0.4999999999999983902, -0.8660254037844395958 ) ) ;
#2400 = CARTESIAN_POINT ( 'NONE',  ( 41.67500000054622689, 24.28113015263587116, 96.68563167572563088 ) ) ;
#2401 = CARTESIAN_POINT ( 'NONE',  ( 24.37500000054622618, 13.07298590277314432, 88.54243821818161564 ) ) ;
#2402 = AXIS2_PLACEMENT_3D ( 'NONE', #6387, #1570, #10251 ) ;
#2403 = CARTESIAN_POINT ( 'NONE',  ( 8.869784206589267583, 15.36130915976373501, 96.70605587419206017 ) ) ;
#2404 = FACE_BOUND ( 'NONE', #9472, .T. ) ;
#2405 = DIRECTION ( 'NONE',  ( 0.000000000000000000, -0.5000000000000012212, -0.8660254037844380415 ) ) ;
#2406 = DIRECTION ( 'NONE',  ( -0.000000000000000000, 1.000000000000000000, 1.224646799147353207E-16 ) ) ;
#2407 = ORIENTED_EDGE ( 'NONE', *, *, #930, .T. ) ;
#2408 = MECHANICAL_DESIGN_GEOMETRIC_PRESENTATION_REPRESENTATION (  '', ( #5855 ), #190 ) ;
#2409 = CARTESIAN_POINT ( 'NONE',  ( -31.74999999999995737, 0.000000000000000000, 0.000000000000000000 ) ) ;
#2410 = ORIENTED_EDGE ( 'NONE', *, *, #6809, .T. ) ;
#2411 = DIRECTION ( 'NONE',  ( -1.000000000000000000, 0.000000000000000000, 0.000000000000000000 ) ) ;
#2412 = ORIENTED_EDGE ( 'NONE', *, *, #4212, .T. ) ;
#2413 = MECHANICAL_DESIGN_GEOMETRIC_PRESENTATION_REPRESENTATION (  '', ( #6059 ), #1803 ) ;
#2414 = EDGE_CURVE ( 'NONE', #12065, #2755, #7092, .T. ) ;
#2415 = CARTESIAN_POINT ( 'NONE',  ( 31.17500000054621978, 26.19570976099943849, 86.29171490190961435 ) ) ;
#2416 = FACE_OUTER_BOUND ( 'NONE', #10341, .T. ) ;
#2417 = CARTESIAN_POINT ( 'NONE',  ( 48.47500000054622404, 13.80429023900056684, 86.29171490190961435 ) ) ;
#2418 = CARTESIAN_POINT ( 'NONE',  ( 34.37500000054622973, 12.34168156654572535, 90.79316153445363113 ) ) ;
#2419 = CARTESIAN_POINT ( 'NONE',  ( 38.89999999999997726, 17.56310227825321135, 83.29316153445363113 ) ) ;
#2420 = EDGE_CURVE ( 'NONE', #4353, #2911, #10527, .T. ) ;
#2421 = CARTESIAN_POINT ( 'NONE',  ( 47.27500000054622831, 27.65831843345427998, 90.79316153445363113 ) ) ;
#2422 = ORIENTED_EDGE ( 'NONE', *, *, #12202, .T. ) ;
#2423 = CARTESIAN_POINT ( 'NONE',  ( 27.95000000109246585, 13.62011893735971135, 95.42841645007781892 ) ) ;
#2424 = CARTESIAN_POINT ( 'NONE',  ( -1.612909136089518691, 45.25592802960594696, 24.94976847917136453 ) ) ;
#2425 = ORIENTED_EDGE ( 'NONE', *, *, #235, .F. ) ;
#2426 = CARTESIAN_POINT ( 'NONE',  ( -2.614082915411372721, 29.67457893774099986, 27.88517181684549229 ) ) ;
#2427 = ORIENTED_EDGE ( 'NONE', *, *, #4592, .F. ) ;
#2428 = EDGE_CURVE ( 'NONE', #6680, #8919, #8109, .T. ) ;
#2429 = DIRECTION ( 'NONE',  ( -1.000000000000000000, -0.000000000000000000, -0.000000000000000000 ) ) ;
#2430 = CARTESIAN_POINT ( 'NONE',  ( 10.00000000000000355, 20.00000000000000355, 109.9999999999999858 ) ) ;
#2431 = CARTESIAN_POINT ( 'NONE',  ( -5.000000000000004441, 20.00000000000000000, 137.5000000000000000 ) ) ;
#2432 = AXIS2_PLACEMENT_3D ( 'NONE', #6978, #10851, #9657 ) ;
#2433 = CYLINDRICAL_SURFACE ( 'NONE', #6562, 7.500000000000000000 ) ;
#2434 = CARTESIAN_POINT ( 'NONE',  ( 24.27500000054622475, 12.34168156654572535, 90.79316153445363113 ) ) ;
#2435 = CARTESIAN_POINT ( 'NONE',  ( 24.37500000054622262, 12.34168156654572535, 90.79316153445363113 ) ) ;
#2436 = DIRECTION ( 'NONE',  ( 0.000000000000000000, 0.000000000000000000, 1.000000000000000000 ) ) ;
#2437 =( BOUNDED_CURVE ( )  B_SPLINE_CURVE ( 2, ( #9695, #4808, #6766, #1816, #1943, #2006, #5703, #11464, #8487, #3716, #2836 ),
 .UNSPECIFIED., .F., .F. ) 
 B_SPLINE_CURVE_WITH_KNOTS ( ( 3, 2, 2, 2, 2, 3 ),
 ( 0.9333333333333333481, 0.9399999999999999467, 0.9466666666666666563, 0.9533333333333333659, 0.9599999999999999645, 0.9666666666666666741 ),
 .UNSPECIFIED. ) 
 CURVE ( )  GEOMETRIC_REPRESENTATION_ITEM ( )  RATIONAL_B_SPLINE_CURVE ( ( 1.000000000000000000, 0.9510565162951535312, 1.000000000000000000, 0.9510565162951535312, 1.000000000000000000, 0.9510565162951535312, 1.000000000000000000, 0.9510565162951535312, 1.000000000000000000, 0.9510565162951535312, 1.000000000000000000 ) ) 
 REPRESENTATION_ITEM ( '' )  );
#2438 = PLANE ( 'NONE',  #9495 ) ;
#2439 = ORIENTED_EDGE ( 'NONE', *, *, #2151, .F. ) ;
#2440 = CARTESIAN_POINT ( 'NONE',  ( 45.35000000109246088, 26.37988106264029398, 95.42841645007781892 ) ) ;
#2441 = ORIENTED_EDGE ( 'NONE', *, *, #7673, .T. ) ;
#2442 = DIRECTION ( 'NONE',  ( 1.000000000000000000, -0.000000000000000000, -0.000000000000000000 ) ) ;
#2443 = AXIS2_PLACEMENT_3D ( 'NONE', #694, #12429, #4438 ) ;
#2444 = VERTEX_POINT ( 'NONE', #12444 ) ;
#2445 = CARTESIAN_POINT ( 'NONE',  ( 0.000000000000000000, 70.00000000000000000, 0.000000000000000000 ) ) ;
#2446 = FACE_OUTER_BOUND ( 'NONE', #2182, .T. ) ;
#2447 = AXIS2_PLACEMENT_3D ( 'NONE', #10998, #3379, #9225 ) ;
#2448 = SURFACE_STYLE_FILL_AREA ( #614 ) ;
#2449 = CARTESIAN_POINT ( 'NONE',  ( -9.869611566543289527, 18.35654797443324782, 22.96945393929722457 ) ) ;
#2450 = ADVANCED_FACE ( 'NONE', ( #6480 ), #4701, .T. ) ;
#2451 = DIRECTION ( 'NONE',  ( 1.000000000000000000, -0.000000000000000000, 0.000000000000000000 ) ) ;
#2452 = PLANE ( 'NONE',  #4756 ) ;
#2453 = CARTESIAN_POINT ( 'NONE',  ( -8.964925771381055952, 15.55726866616962134, 26.52653170654884107 ) ) ;
#2454 = CARTESIAN_POINT ( 'NONE',  ( 2.290457103807213457, 29.73981914200485477, 24.89699738223682246 ) ) ;
#2455 = CARTESIAN_POINT ( 'NONE',  ( 0.000000000000000000, 139.9999999999999716, 0.000000000000000000 ) ) ;
#2456 = ORIENTED_EDGE ( 'NONE', *, *, #4472, .T. ) ;
#2457 = ITEM_DEFINED_TRANSFORMATION ( 'NONE', 'NONE', #8587,  #9021 ) ;
#2458 = CARTESIAN_POINT ( 'NONE',  ( 4.491750101222253377, 47.77928715861156661, 24.59350609687774281 ) ) ;
#2459 = CARTESIAN_POINT ( 'NONE',  ( 1.614235646224727372, 54.74352724365349587, 24.94966740611544509 ) ) ;
#2460 = CARTESIAN_POINT ( 'NONE',  ( 44.57500000054622546, 13.80429023900056684, 86.29171490190961435 ) ) ;
#2461 = CARTESIAN_POINT ( 'NONE',  ( 29.47500000054622404, 26.19570976099943849, 95.29460816699764791 ) ) ;
#2462 = CARTESIAN_POINT ( 'NONE',  ( 9.983753628317437290, 19.33993981085001579, -22.91999041428549688 ) ) ;
#2463 = FACE_OUTER_BOUND ( 'NONE', #1916, .T. ) ;
#2464 = DIRECTION ( 'NONE',  ( -1.000000000000000000, -0.000000000000000000, -0.000000000000000000 ) ) ;
#2465 = DIRECTION ( 'NONE',  ( 0.000000000000000000, -1.224646799147353207E-16, 1.000000000000000000 ) ) ;
#2466 = B_SPLINE_CURVE_WITH_KNOTS ( 'NONE', 3,
 ( #11905, #1125, #8917, #7969, #3968, #6004, #8789, #8035, #6944, #7843, #5877, #3017, #10811, #6883, #2126, #7073, #6069, #9876, #5814, #4862 ),
 .UNSPECIFIED., .F., .F.,
 ( 4, 2, 2, 2, 2, 2, 2, 2, 2, 4 ),
 ( 0.02350824016915415912, 0.02448716854195917558, 0.02546609691476419204, 0.02644502528756920851, 0.02693448947397171500, 0.02742395366037422497, 0.02840288203317925531, 0.02938181040598428218, 0.03036073877878931251, 0.03133966715159434285 ),
 .UNSPECIFIED. ) ;
#2467 = ORIENTED_EDGE ( 'NONE', *, *, #8533, .F. ) ;
#2468 = EDGE_CURVE ( 'NONE', #6417, #1603, #4514, .T. ) ;
#2469 = DIRECTION ( 'NONE',  ( 1.000000000000000000, -0.000000000000000000, -0.000000000000000000 ) ) ;
#2470 = ORIENTED_EDGE ( 'NONE', *, *, #5986, .T. ) ;
#2471 = LINE ( 'NONE', #6346, #1836 ) ;
#2472 = EDGE_LOOP ( 'NONE', ( #3080, #8282, #4849, #12524 ) ) ;
#2473 = PRODUCT_RELATED_PRODUCT_CATEGORY ( 'part', '', ( #8 ) ) ;
#2474 = EDGE_CURVE ( 'NONE', #5241, #12263, #1951, .T. ) ;
#2475 = CARTESIAN_POINT ( 'NONE',  ( 31.97500000054622760, 17.63344945572769973, 98.07665518445361386 ) ) ;
#2476 = DIRECTION ( 'NONE',  ( -0.7071067811865452413, 0.000000000000000000, 0.7071067811865497932 ) ) ;
#2477 = CARTESIAN_POINT ( 'NONE',  ( 45.87500000054622973, 17.63344945572769973, 98.07665518445361386 ) ) ;
#2478 = CARTESIAN_POINT ( 'NONE',  ( 33.37500000054621552, 27.65831843345427998, 90.79316153445363113 ) ) ;
#2479 = CARTESIAN_POINT ( 'NONE',  ( 35.89999999999998437, 22.43689772174679575, 98.29316153445363113 ) ) ;
#2480 = CARTESIAN_POINT ( 'NONE',  ( 6.112888882359681197, 27.94072674827362590, 24.24745615746033423 ) ) ;
#2481 = CARTESIAN_POINT ( 'NONE',  ( 42.47500000054622404, 13.80429023900056684, 86.29171490190961435 ) ) ;
#2482 = ORIENTED_EDGE ( 'NONE', *, *, #11027, .F. ) ;
#2483 = CARTESIAN_POINT ( 'NONE',  ( 27.75000000109246301, 17.56310227825320425, 98.29316153445363113 ) ) ;
#2484 = CARTESIAN_POINT ( 'NONE',  ( -3.051014581595654640, 46.02544827001062089, 24.81461801464184802 ) ) ;
#2485 = VERTEX_POINT ( 'NONE', #12198 ) ;
#2486 = CARTESIAN_POINT ( 'NONE',  ( -0.6612821460558259146, 29.98364310583667347, 27.99414546905236989 ) ) ;
#2487 = ORIENTED_EDGE ( 'NONE', *, *, #8314, .T. ) ;
#2488 = CIRCLE ( 'NONE', #9390, 5.057500000000000107 ) ;
#2489 = CARTESIAN_POINT ( 'NONE',  ( 22.99999999999998934, 20.00000000000000355, 83.29316153445364534 ) ) ;
#2490 = CARTESIAN_POINT ( 'NONE',  ( 27.49999999999999645, 20.00000000000000355, 170.0000119999999697 ) ) ;
#2491 = EDGE_CURVE ( 'NONE', #6721, #11614, #6887, .T. ) ;
#2492 = CARTESIAN_POINT ( 'NONE',  ( -31.74999999999995737, 0.000000000000000000, 5.999999999999999112 ) ) ;
#2493 = B_SPLINE_CURVE_WITH_KNOTS ( 'NONE', 3,
 ( #8522, #3757, #6611, #4591, #9422, #9483, #723, #7637, #8463, #11502, #10544, #6046, #978, #7698, #6925, #10863, #4008, #8710, #8898, #7885, #10792, #5922, #2106, #12518 ),
 .UNSPECIFIED., .F., .F.,
 ( 4, 2, 2, 2, 2, 2, 2, 2, 2, 2, 2, 4 ),
 ( 5.438949063372056100E-19, 0.001975691086292785757, 0.002963536629439178418, 0.003951382172585572380, 0.005927073258878355969, 0.006914918802024747763, 0.007902764345171137822, 0.009878455431463928349, 0.01185414651775671888, 0.01284199206090311240, 0.01382983760404950767, 0.01580552869034228605 ),
 .UNSPECIFIED. ) ;
#2494 = CARTESIAN_POINT ( 'NONE',  ( 32.65000000109246514, 20.00000000000000355, 83.29316153445364534 ) ) ;
#2495 =( BOUNDED_CURVE ( )  B_SPLINE_CURVE ( 3, ( #11374, #9166, #11311, #4521 ),
 .UNSPECIFIED., .F., .F. ) 
 B_SPLINE_CURVE_WITH_KNOTS ( ( 4, 4 ),
 ( 1.570796326794896558, 2.871659857756389655 ),
 .UNSPECIFIED. ) 
 CURVE ( )  GEOMETRIC_REPRESENTATION_ITEM ( )  RATIONAL_B_SPLINE_CURVE ( ( 1.000000000000000000, 0.8638816171694809753, 0.8638816171694809753, 1.000000000000000000 ) ) 
 REPRESENTATION_ITEM ( '' )  );
#2496 = CARTESIAN_POINT ( 'NONE',  ( 25.77500000054622831, 20.00000000000000355, 98.07665518445361386 ) ) ;
#2497 = CARTESIAN_POINT ( 'NONE',  ( 28.07500000054622546, 15.71886984736413417, 96.68563167572563088 ) ) ;
#2498 = AXIS2_PLACEMENT_3D ( 'NONE', #7592, #12472, #2829 ) ;
#2499 = DIRECTION ( 'NONE',  ( 1.000000000000000000, -0.000000000000000000, -0.000000000000000000 ) ) ;
#2500 = EDGE_CURVE ( 'NONE', #2989, #315, #4579, .T. ) ;
#2501 = DIRECTION ( 'NONE',  ( 0.000000000000000000, 1.000000000000000000, -1.295896757998781374E-15 ) ) ;
#2502 = ORIENTED_EDGE ( 'NONE', *, *, #1701, .F. ) ;
#2503 = CARTESIAN_POINT ( 'NONE',  ( 44.25000000109246656, 12.86707612778636012, 88.47553407664152303 ) ) ;
#2504 = PRESENTATION_STYLE_ASSIGNMENT (( #10065 ) ) ;
#2505 = EDGE_LOOP ( 'NONE', ( #3068, #6088, #2939, #5402, #817 ) ) ;
#2506 = CARTESIAN_POINT ( 'NONE',  ( 46.99999999999998579, 20.00000000000000355, 83.29316153445364534 ) ) ;
#2507 = ORIENTED_EDGE ( 'NONE', *, *, #1677, .F. ) ;
#2508 = EDGE_CURVE ( 'NONE', #5989, #8756, #5481, .T. ) ;
#2509 = CARTESIAN_POINT ( 'NONE',  ( -10.00000000000000355, 20.00000000000000355, -22.91287847477919826 ) ) ;
#2510 = VECTOR ( 'NONE', #11080, 999.9999999999998863 ) ;
#2511 = CARTESIAN_POINT ( 'NONE',  ( -9.481431770954213079, 23.24517152888003224, 23.13387126485941536 ) ) ;
#2512 = CONICAL_SURFACE ( 'NONE', #3326, 5.057500000000000107, 1.047197551196592302 ) ;
#2513 = EDGE_CURVE ( 'NONE', #6066, #5525, #10418, .T. ) ;
#2514 = CARTESIAN_POINT ( 'NONE',  ( 5.000000000000000000, 50.33107439471904598, 24.49489742783178770 ) ) ;
#2515 = CARTESIAN_POINT ( 'NONE',  ( -1.652347697333065968, 10.13198208422932467, 24.94742907234073215 ) ) ;
#2516 = FACE_OUTER_BOUND ( 'NONE', #2630, .T. ) ;
#2517 = LINE ( 'NONE', #4483, #3135 ) ;
#2518 = CARTESIAN_POINT ( 'NONE',  ( 0.6000000000000033085, 1.102182119232617714E-15, -9.000000000000000000 ) ) ;
#2519 = FACE_OUTER_BOUND ( 'NONE', #6320, .T. ) ;
#2520 = AXIS2_PLACEMENT_3D ( 'NONE', #3090, #6958, #7856 ) ;
#2521 = FACE_OUTER_BOUND ( 'NONE', #869, .T. ) ;
#2522 = ORIENTED_EDGE ( 'NONE', *, *, #10958, .T. ) ;
#2523 = DIRECTION ( 'NONE',  ( 0.000000000000000000, 0.000000000000000000, -1.000000000000000000 ) ) ;
#2524 = VECTOR ( 'NONE', #4458, 1000.000000000000000 ) ;
#2525 = CARTESIAN_POINT ( 'NONE',  ( 4.741482771685880948, 51.61996731904482516, 24.54657867284130646 ) ) ;
#2526 = CARTESIAN_POINT ( 'NONE',  ( 38.07500000054622546, 15.71886984736413417, 96.68563167572563088 ) ) ;
#2527 = CARTESIAN_POINT ( 'NONE',  ( 26.27500000054622475, 12.34168156654572357, 90.79316153445363113 ) ) ;
#2528 = CARTESIAN_POINT ( 'NONE',  ( 6.732131639182266092, 12.60512992570006929, 92.06969329359783671 ) ) ;
#2529 = LINE ( 'NONE', #3421, #11092 ) ;
#2530 = FACE_OUTER_BOUND ( 'NONE', #2673, .T. ) ;
#2531 = EDGE_LOOP ( 'NONE', ( #3024, #8191, #7057 ) ) ;
#2532 = DIRECTION ( 'NONE',  ( 1.000000000000000000, -0.000000000000000000, -0.000000000000000000 ) ) ;
#2533 = ORIENTED_EDGE ( 'NONE', *, *, #10351, .F. ) ;
#2534 = CARTESIAN_POINT ( 'NONE',  ( 89.17200000000001125, 0.000000000000000000, 5.000000000000001776 ) ) ;
#2535 = AXIS2_PLACEMENT_3D ( 'NONE', #10508, #874, #8429 ) ;
#2536 = ADVANCED_FACE ( 'NONE', ( #8450 ), #6683, .F. ) ;
#2537 = CARTESIAN_POINT ( 'NONE',  ( 0.000000000000000000, 0.000000000000000000, 379.9999999999999432 ) ) ;
#2538 = CARTESIAN_POINT ( 'NONE',  ( 30.07500000054622546, 15.71886984736413417, 96.68563167572563088 ) ) ;
#2539 = DIRECTION ( 'NONE',  ( 0.000000000000000000, -0.5000000000000011102, -0.8660254037844380415 ) ) ;
#2540 = AXIS2_PLACEMENT_3D ( 'NONE', #3055, #271, #6917 ) ;
#2541 = CARTESIAN_POINT ( 'NONE',  ( 42.97500000054623115, 24.28113015263587471, 84.90069139318163138 ) ) ;
#2542 = CARTESIAN_POINT ( 'NONE',  ( 34.09999999999998721, 17.56310227825320425, 98.29316153445363113 ) ) ;
#2543 = CARTESIAN_POINT ( 'NONE',  ( 9.867555937047535863, 21.65500574101911724, 22.97033549711487410 ) ) ;
#2544 = CARTESIAN_POINT ( 'NONE',  ( 37.87500000054622262, 17.63344945572769973, 98.07665518445361386 ) ) ;
#2545 = ORIENTED_EDGE ( 'NONE', *, *, #11307, .F. ) ;
#2546 = CARTESIAN_POINT ( 'NONE',  ( 45.57500000054622546, 24.28113015263587116, 96.68563167572563088 ) ) ;
#2547 = CARTESIAN_POINT ( 'NONE',  ( 28.65000000109246514, 20.00000000000000355, 83.29316153445364534 ) ) ;
#2548 = ORIENTED_EDGE ( 'NONE', *, *, #6876, .F. ) ;
#2549 = CARTESIAN_POINT ( 'NONE',  ( 3.429011038972528284E-15, 30.00000000000001066, 28.00000000000000355 ) ) ;
#2550 = VERTEX_POINT ( 'NONE', #1966 ) ;
#2551 = DIRECTION ( 'NONE',  ( 0.000000000000000000, 0.000000000000000000, 1.000000000000000000 ) ) ;
#2552 = CARTESIAN_POINT ( 'NONE',  ( 48.65000000109246514, 20.00000000000000355, 83.29316153445364534 ) ) ;
#2553 = CARTESIAN_POINT ( 'NONE',  ( -27.49999999999999645, 12.50000000000001066, 145.0000000000000000 ) ) ;
#2554 = CARTESIAN_POINT ( 'NONE',  ( 25.99999999999998934, 20.00000000000000355, 98.29316153445363113 ) ) ;
#2555 = ADVANCED_FACE ( 'NONE', ( #11615 ), #8717, .F. ) ;
#2556 = CARTESIAN_POINT ( 'NONE',  ( 21.17500000054623044, 26.92701409722686634, 88.54243821818162985 ) ) ;
#2557 = CARTESIAN_POINT ( 'NONE',  ( 23.57500000054622546, 26.19570976099943493, 95.29460816699764791 ) ) ;
#2558 = VECTOR ( 'NONE', #2083, 1000.000000000000000 ) ;
#2559 = CARTESIAN_POINT ( 'NONE',  ( 41.79999999999999005, 24.40838939219354842, 96.86078899226572503 ) ) ;
#2560 = DIRECTION ( 'NONE',  ( -1.000000000000000000, -0.000000000000000000, -0.000000000000000000 ) ) ;
#2561 = ORIENTED_EDGE ( 'NONE', *, *, #2650, .T. ) ;
#2562 = CARTESIAN_POINT ( 'NONE',  ( 40.15000000109245804, 12.11403331821300533, 90.79316153445363113 ) ) ;
#2563 =( NAMED_UNIT ( * ) SI_UNIT ( $, .STERADIAN. ) SOLID_ANGLE_UNIT ( ) );
#2564 = ORIENTED_EDGE ( 'NONE', *, *, #9879, .T. ) ;
#2565 = CARTESIAN_POINT ( 'NONE',  ( -2.000000000000015543, 20.00000000000000355, 83.29316153445364534 ) ) ;
#2566 = VERTEX_POINT ( 'NONE', #10779 ) ;
#2567 = CARTESIAN_POINT ( 'NONE',  ( 0.6549955759030559044, 54.96769473000979644, 20.99223993983284586 ) ) ;
#2568 = VECTOR ( 'NONE', #12453, 1000.000000000000000 ) ;
#2569 = CARTESIAN_POINT ( 'NONE',  ( 92.00000000000000000, 0.000000000000000000, 0.000000000000000000 ) ) ;
#2570 = ADVANCED_FACE ( 'NONE', ( #2161 ), #5969, .T. ) ;
#2571 = CARTESIAN_POINT ( 'NONE',  ( 20.37500000054622618, 13.07298590277314432, 88.54243821818161564 ) ) ;
#2572 = EDGE_CURVE ( 'NONE', #2798, #12151, #964, .T. ) ;
#2573 = LINE ( 'NONE', #9187, #5982 ) ;
#2574 = CARTESIAN_POINT ( 'NONE',  ( -5.000000000000000000, 49.67307781155022894, 20.39607805437114507 ) ) ;
#2575 = CARTESIAN_POINT ( 'NONE',  ( -9.352703157270289225, 16.44582563935068009, 18.80282705866110149 ) ) ;
#2576 = ADVANCED_FACE ( 'NONE', ( #1157 ), #11345, .T. ) ;
#2577 = DIRECTION ( 'NONE',  ( -1.000000000000000000, -0.000000000000000000, -0.000000000000000000 ) ) ;
#2578 = CARTESIAN_POINT ( 'NONE',  ( 27.87500000054622618, 17.63344945572769973, 98.07665518445361386 ) ) ;
#2579 = AXIS2_PLACEMENT_3D ( 'NONE', #10387, #3665, #5521 ) ;
#2580 = CARTESIAN_POINT ( 'NONE',  ( 3.239919941357241040, 29.46629152487073000, 24.79118428027058840 ) ) ;
#2581 = CARTESIAN_POINT ( 'NONE',  ( -4.743460743378065558, 51.61424263853129446, 24.54619549801029166 ) ) ;
#2582 = ORIENTED_EDGE ( 'NONE', *, *, #747, .T. ) ;
#2583 = FACE_OUTER_BOUND ( 'NONE', #10214, .T. ) ;
#2584 = VECTOR ( 'NONE', #6211, 1000.000000000000000 ) ;
#2585 = CARTESIAN_POINT ( 'NONE',  ( -28.50000000000001066, 69.50000000000000000, 146.8533255156881978 ) ) ;
#2586 = CARTESIAN_POINT ( 'NONE',  ( 39.37500000054622973, 26.92701409722686634, 93.04388485072563242 ) ) ;
#2587 = CARTESIAN_POINT ( 'NONE',  ( 37.07500000054622546, 24.28113015263587471, 84.90069139318163138 ) ) ;
#2588 = CARTESIAN_POINT ( 'NONE',  ( 29.87500000054622618, 17.63344945572769973, 98.07665518445361386 ) ) ;
#2589 = CARTESIAN_POINT ( 'NONE',  ( 8.035382134961579936, 14.03808006457184199, 95.36761081598396572 ) ) ;
#2590 = CARTESIAN_POINT ( 'NONE',  ( 1.614504882520976681, 45.25664461204844713, 24.94963714481321304 ) ) ;
#2591 = DIRECTION ( 'NONE',  ( 0.000000000000000000, -0.5000000000000009992, -0.8660254037844380415 ) ) ;
#2592 = CYLINDRICAL_SURFACE ( 'NONE', #5060, 7.500000000000007105 ) ;
#2593 = AXIS2_PLACEMENT_3D ( 'NONE', #6469, #11292, #2664 ) ;
#2594 = ORIENTED_EDGE ( 'NONE', *, *, #905, .T. ) ;
#2595 = FACE_OUTER_BOUND ( 'NONE', #7906, .T. ) ;
#2596 = EDGE_LOOP ( 'NONE', ( #5876, #9536, #2058, #3144 ) ) ;
#2597 = CARTESIAN_POINT ( 'NONE',  ( -50.00000000000001421, 92.00000000000000000, 166.8533255156881694 ) ) ;
#2598 = APPLICATION_PROTOCOL_DEFINITION ( 'draft international standard', 'automotive_design', 1998, #3909 ) ;
#2599 = AXIS2_PLACEMENT_3D ( 'NONE', #875, #9572, #1756 ) ;
#2600 = CARTESIAN_POINT ( 'NONE',  ( 29.87500000054622618, 20.00000000000000355, 98.07665518445361386 ) ) ;
#2601 = CARTESIAN_POINT ( 'NONE',  ( 29.05000000109246727, 27.13292387221364876, 88.47553407664153724 ) ) ;
#2602 = CARTESIAN_POINT ( 'NONE',  ( 44.07500000054623257, 13.80429023900056507, 95.29460816699764791 ) ) ;
#2603 = VECTOR ( 'NONE', #4720, 1000.000000000000000 ) ;
#2604 = CARTESIAN_POINT ( 'NONE',  ( 33.87500000054622262, 20.00000000000000355, 98.07665518445361386 ) ) ;
#2605 = CARTESIAN_POINT ( 'NONE',  ( 31.39999999999998437, 27.13292387221364876, 88.47553407664153724 ) ) ;
#2606 = CARTESIAN_POINT ( 'NONE',  ( -19.99999999999999645, 20.00000000000000355, 99.99999999999997158 ) ) ;
#2607 = ADVANCED_FACE ( 'NONE', ( #5846 ), #8698, .F. ) ;
#2608 = CARTESIAN_POINT ( 'NONE',  ( 41.37500000054622262, 26.92701409722686634, 93.04388485072563242 ) ) ;
#2609 = EDGE_LOOP ( 'NONE', ( #8452, #7685, #11325, #345, #5171 ) ) ;
#2610 = CARTESIAN_POINT ( 'NONE',  ( 49.77500000054622831, 20.00000000000000355, 98.07665518445361386 ) ) ;
#2611 = DIRECTION ( 'NONE',  ( -0.000000000000000000, -0.000000000000000000, 1.000000000000000000 ) ) ;
#2612 = VERTEX_POINT ( 'NONE', #10654 ) ;
#2613 =( REPRESENTATION_RELATIONSHIP ('NONE','NONE', #4262, #10013 ) REPRESENTATION_RELATIONSHIP_WITH_TRANSFORMATION ( #4883 )SHAPE_REPRESENTATION_RELATIONSHIP( ) );
#2614 = CARTESIAN_POINT ( 'NONE',  ( -31.74999999999995737, 0.000000000000000000, 0.000000000000000000 ) ) ;
#2615 = VERTEX_POINT ( 'NONE', #5019 ) ;
#2616 = VECTOR ( 'NONE', #8531, 1000.000000000000000 ) ;
#2617 = CARTESIAN_POINT ( 'NONE',  ( 41.85000000109246798, 15.59161060780645691, 96.86078899226572503 ) ) ;
#2618 = CARTESIAN_POINT ( 'NONE',  ( 21.45000000109246230, 24.40838939219354842, 96.86078899226572503 ) ) ;
#2619 = B_SPLINE_CURVE_WITH_KNOTS ( 'NONE', 3,
 ( #1531, #3490, #12068, #6351, #5405, #9276, #580, #4446, #1415, #9977, #12190, #7361, #6108, #1287, #5160, #338, #4201, #3247 ),
 .UNSPECIFIED., .F., .F.,
 ( 4, 2, 2, 2, 2, 2, 2, 2, 4 ),
 ( 0.02349641915568531983, 0.02447480192481506570, 0.02545318469394481503, 0.02643156746307456090, 0.02740995023220430676, 0.02838833300133405610, 0.02936671577046380197, 0.03034509853959355130, 0.03132348130872329717 ),
 .UNSPECIFIED. ) ;
#2620 = DIRECTION ( 'NONE',  ( 0.000000000000000000, 0.000000000000000000, -1.000000000000000000 ) ) ;
#2621 = DIRECTION ( 'NONE',  ( -1.000000000000000000, 0.000000000000000000, 0.000000000000000000 ) ) ;
#2622 = CARTESIAN_POINT ( 'NONE',  ( 21.77500000054622831, 20.00000000000000355, 98.07665518445361386 ) ) ;
#2623 = CARTESIAN_POINT ( 'NONE',  ( 22.77500000054622475, 17.63344945572770328, 83.50966788445364841 ) ) ;
#2624 = DIRECTION ( 'NONE',  ( 0.000000000000000000, 0.000000000000000000, 1.000000000000000000 ) ) ;
#2625 = VECTOR ( 'NONE', #6308, 1000.000000000000000 ) ;
#2626 = DIRECTION ( 'NONE',  ( 0.000000000000000000, -1.000000000000000000, 1.039664082171044875E-15 ) ) ;
#2627 = ORIENTED_EDGE ( 'NONE', *, *, #952, .F. ) ;
#2628 = CARTESIAN_POINT ( 'NONE',  ( 35.55000000109245661, 22.43689772174679575, 98.29316153445363113 ) ) ;
#2629 = CARTESIAN_POINT ( 'NONE',  ( 7.297088297540795132, 13.15481214220262274, 23.91253034306283354 ) ) ;
#2630 = EDGE_LOOP ( 'NONE', ( #8653, #6116, #9080, #4636, #11908 ) ) ;
#2631 = CARTESIAN_POINT ( 'NONE',  ( 47.99999999999998579, 20.00000000000000355, 98.29316153445363113 ) ) ;
#2632 = ADVANCED_FACE ( 'NONE', ( #11802 ), #9718, .F. ) ;
#2633 = ORIENTED_EDGE ( 'NONE', *, *, #5487, .F. ) ;
#2634 = AXIS2_PLACEMENT_3D ( 'NONE', #10717, #9844, #3935 ) ;
#2635 = CARTESIAN_POINT ( 'NONE',  ( 3.763812309688671753, 53.30741636328656341, 20.66126648110244801 ) ) ;
#2636 = CARTESIAN_POINT ( 'NONE',  ( 9.670754941354928746, 17.37006389387946470, -18.64131299320824198 ) ) ;
#2637 = DIRECTION ( 'NONE',  ( 1.000000000000000000, -0.000000000000000000, -0.000000000000000000 ) ) ;
#2638 = ADVANCED_FACE ( 'NONE', ( #7686 ), #3996, .F. ) ;
#2639 = DIRECTION ( 'NONE',  ( 0.000000000000000000, 0.000000000000000000, -1.000000000000000000 ) ) ;
#2640 = DIRECTION ( 'NONE',  ( -0.000000000000000000, -1.000000000000000000, -0.000000000000000000 ) ) ;
#2641 = CIRCLE ( 'NONE', #7716, 7.500000000000000000 ) ;
#2642 = DIRECTION ( 'NONE',  ( 1.000000000000000000, -0.000000000000000000, -0.000000000000000000 ) ) ;
#2643 = CARTESIAN_POINT ( 'NONE',  ( 47.95000000109246230, 13.62011893735970958, 95.42841645007781892 ) ) ;
#2644 = CARTESIAN_POINT ( 'NONE',  ( 47.47500000054622404, 26.92701409722686634, 93.04388485072563242 ) ) ;
#2645 = DIRECTION ( 'NONE',  ( 0.000000000000000000, 0.000000000000000000, -1.000000000000000000 ) ) ;
#2646 = CARTESIAN_POINT ( 'NONE',  ( 5.000000000000000000, -4.685197434473812983, 6.938893903907228378E-15 ) ) ;
#2647 = ORIENTED_EDGE ( 'NONE', *, *, #10368, .T. ) ;
#2648 = AXIS2_PLACEMENT_3D ( 'NONE', #9333, #1586, #12304 ) ;
#2649 = DIRECTION ( 'NONE',  ( 1.000000000000000000, 0.000000000000000000, 0.000000000000000000 ) ) ;
#2650 = EDGE_CURVE ( 'NONE', #918, #9719, #3640, .T. ) ;
#2651 = B_SPLINE_CURVE_WITH_KNOTS ( 'NONE', 3,
 ( #7651, #12410, #8727, #2764, #3588, #11584, #7462, #6693, #11457, #4861, #3649, #1684, #1870, #5813, #2828, #7527, #3841, #10561, #5752, #6626 ),
 .UNSPECIFIED., .F., .F.,
 ( 4, 2, 2, 2, 2, 2, 2, 2, 2, 4 ),
 ( 8.418992706677550310E-19, 0.0009792220048825109237, 0.001468833007323765844, 0.001958444009765020980, 0.002937666014647530820, 0.003916888019530041093, 0.004896110024412551366, 0.005875332029295060772, 0.006854554034177571045, 0.007833776039060080451 ),
 .UNSPECIFIED. ) ;
#2652 = DIRECTION ( 'NONE',  ( -0.5000000000000034417, 1.060575238724904696E-16, -0.8660254037844367092 ) ) ;
#2653 = CARTESIAN_POINT ( 'NONE',  ( 35.27500000054622831, 27.65831843345427998, 90.79316153445363113 ) ) ;
#2654 = CARTESIAN_POINT ( 'NONE',  ( 35.07500000054622546, 24.28113015263587471, 84.90069139318163138 ) ) ;
#2655 = CARTESIAN_POINT ( 'NONE',  ( 20.67500000054622689, 17.63344945572770328, 83.50966788445364841 ) ) ;
#2656 = DIRECTION ( 'NONE',  ( 0.000000000000000000, 0.000000000000000000, 1.000000000000000000 ) ) ;
#2657 = DIRECTION ( 'NONE',  ( -0.000000000000000000, -0.000000000000000000, 1.000000000000000000 ) ) ;
#2658 = FACE_OUTER_BOUND ( 'NONE', #10327, .T. ) ;
#2659 = LINE ( 'NONE', #1758, #5470 ) ;
#2660 = EDGE_CURVE ( 'NONE', #1521, #8006, #6722, .T. ) ;
#2661 = VECTOR ( 'NONE', #140, 1000.000000000000000 ) ;
#2662 = DIRECTION ( 'NONE',  ( 1.000000000000000000, 0.000000000000000000, 0.000000000000000000 ) ) ;
#2663 = ORIENTED_EDGE ( 'NONE', *, *, #1938, .F. ) ;
#2664 = DIRECTION ( 'NONE',  ( 0.000000000000000000, 0.000000000000000000, -1.000000000000000000 ) ) ;
#2665 = DIRECTION ( 'NONE',  ( 0.000000000000000000, 0.000000000000000000, -1.000000000000000000 ) ) ;
#2666 = CARTESIAN_POINT ( 'NONE',  ( 24.87500000054622262, 20.00000000000000355, 83.50966788445364841 ) ) ;
#2667 = CARTESIAN_POINT ( 'NONE',  ( 6.000000000000000000, 2.919948986426526005, -5.057500000000003659 ) ) ;
#2668 = CARTESIAN_POINT ( 'NONE',  ( 43.57500000054623257, 24.28113015263587116, 96.68563167572563088 ) ) ;
#2669 = CARTESIAN_POINT ( 'NONE',  ( 26.77500000054622475, 17.63344945572770328, 83.50966788445364841 ) ) ;
#2670 = CARTESIAN_POINT ( 'NONE',  ( 27.09999999999999076, 22.43689772174679575, 83.29316153445363113 ) ) ;
#2671 = CARTESIAN_POINT ( 'NONE',  ( 3.239919941357241040, 29.46629152487073000, 24.79118428027058840 ) ) ;
#2672 = CARTESIAN_POINT ( 'NONE',  ( 39.57500000054622546, 24.28113015263587116, 96.68563167572563088 ) ) ;
#2673 = EDGE_LOOP ( 'NONE', ( #4096, #2288, #2487, #12201, #10564 ) ) ;
#2674 = CARTESIAN_POINT ( 'NONE',  ( 47.37500000054622973, 26.92701409722686634, 93.04388485072563242 ) ) ;
#2675 = CARTESIAN_POINT ( 'NONE',  ( 3.024050948510435495E-21, 45.00000000000000711, -21.00000000000000000 ) ) ;
#2676 = ORIENTED_EDGE ( 'NONE', *, *, #5792, .T. ) ;
#2677 = CARTESIAN_POINT ( 'NONE',  ( 9.656537145003039058, 17.38065509551421073, 18.64841052569367719 ) ) ;
#2678 = EDGE_LOOP ( 'NONE', ( #6072, #9675 ) ) ;
#2679 = CARTESIAN_POINT ( 'NONE',  ( 0.3338900548043083893, 30.00000000000001066, -25.00000000000000355 ) ) ;
#2680 = CARTESIAN_POINT ( 'NONE',  ( -0.3313438815916917579, 54.99999999999998579, -25.00000000000000000 ) ) ;
#2681 = CARTESIAN_POINT ( 'NONE',  ( -20.27158385259952667, 18.00000000000000355, 152.2284161474004520 ) ) ;
#2682 = CARTESIAN_POINT ( 'NONE',  ( 43.47500000054622404, 26.92701409722686634, 93.04388485072563242 ) ) ;
#2683 = DIRECTION ( 'NONE',  ( 8.659560562354927928E-17, -0.7071067811865479058, 0.7071067811865471286 ) ) ;
#2684 = CARTESIAN_POINT ( 'NONE',  ( 25.07500000054623257, 26.19570976099943493, 86.29171490190961435 ) ) ;
#2685 = CARTESIAN_POINT ( 'NONE',  ( 48.29999999999999005, 13.62011893735971135, 95.42841645007781892 ) ) ;
#2686 = DIRECTION ( 'NONE',  ( 1.000000000000000000, -0.000000000000000000, -0.000000000000000000 ) ) ;
#2687 = CARTESIAN_POINT ( 'NONE',  ( -5.000000000000000000, 50.00000000000000000, 24.49489742783178414 ) ) ;
#2688 = ORIENTED_EDGE ( 'NONE', *, *, #1952, .T. ) ;
#2689 = B_SPLINE_CURVE_WITH_KNOTS ( 'NONE', 3,
 ( #4156, #8385, #1537, #6128, #7492, #2671, #9218, #10339, #4385, #11902, #6415, #2480, #11234, #9281, #3208, #6534, #1714, #5537, #1656, #9998, #4574, #12315, #6356, #2543, #584, #11364, #4450, #8328 ),
 .UNSPECIFIED., .F., .F.,
 ( 4, 2, 2, 2, 2, 2, 2, 2, 2, 2, 2, 2, 2, 4 ),
 ( 0.04738593773884331589, 0.04935840384251231894, 0.05034463689434681699, 0.05133086994618132198, 0.05231710299801582004, 0.05330333604985031809, 0.05527580215351931420, 0.05626203520535381225, 0.05724826825718831030, 0.05922073436085731335, 0.06020696741269181834, 0.06119320046452632333, 0.06217943351636082833, 0.06316566656819533332 ),
 .UNSPECIFIED. ) ;
#2690 = VECTOR ( 'NONE', #6588, 1000.000000000000000 ) ;
#2691 = CARTESIAN_POINT ( 'NONE',  ( 38.55000000109247082, 17.56310227825321135, 83.29316153445363113 ) ) ;
#2692 = LINE ( 'NONE', #4532, #1817 ) ;
#2693 = ORIENTED_EDGE ( 'NONE', *, *, #8703, .T. ) ;
#2694 = FACE_BOUND ( 'NONE', #8794, .T. ) ;
#2695 = VERTEX_POINT ( 'NONE', #10589 ) ;
#2696 = CARTESIAN_POINT ( 'NONE',  ( 4.967355519288257248, 50.65829285064151577, 20.40416061862378072 ) ) ;
#2697 = CARTESIAN_POINT ( 'NONE',  ( 4.171089004654445986, 10.90545738055656066, -20.58391839369968324 ) ) ;
#2698 = ADVANCED_FACE ( 'NONE', ( #11744 ), #1901, .T. ) ;
#2699 = CARTESIAN_POINT ( 'NONE',  ( 3.061617454482527662E-15, 30.00000000000001066, 25.00000000000000000 ) ) ;
#2700 = FACE_OUTER_BOUND ( 'NONE', #8576, .T. ) ;
#2701 = LINE ( 'NONE', #11336, #3226 ) ;
#2702 = ORIENTED_EDGE ( 'NONE', *, *, #6023, .F. ) ;
#2703 = CARTESIAN_POINT ( 'NONE',  ( 90.00000000000000000, 0.000000000000000000, 0.000000000000000000 ) ) ;
#2704 = CARTESIAN_POINT ( 'NONE',  ( 47.85000000109246088, 15.59161060780645691, 96.86078899226572503 ) ) ;
#2705 = CARTESIAN_POINT ( 'NONE',  ( 49.17500000054622689, 26.19570976099943493, 86.29171490190961435 ) ) ;
#2706 = CARTESIAN_POINT ( 'NONE',  ( 53.99999999999999289, 20.00000000000000711, 170.9999999999999716 ) ) ;
#2707 = CONICAL_SURFACE ( 'NONE', #8996, 25.00000000000000355, 0.7853981633974482790 ) ;
#2708 = CARTESIAN_POINT ( 'NONE',  ( 36.65000000109245804, 20.00000000000000355, 83.29316153445364534 ) ) ;
#2709 = VERTEX_POINT ( 'NONE', #3109 ) ;
#2710 = ADVANCED_FACE ( 'NONE', ( #6913 ), #11682, .F. ) ;
#2711 = ORIENTED_EDGE ( 'NONE', *, *, #10237, .F. ) ;
#2712 = CARTESIAN_POINT ( 'NONE',  ( -10.00000000000000888, 20.66452866687815160, -18.46618531261939822 ) ) ;
#2713 = CARTESIAN_POINT ( 'NONE',  ( 0.000000000000000000, 0.000000000000000000, 0.000000000000000000 ) ) ;
#2714 = CARTESIAN_POINT ( 'NONE',  ( 36.27500000054622120, 13.07298590277314254, 93.04388485072563242 ) ) ;
#2716 = ADVANCED_FACE ( 'NONE', ( #4894 ), #4661, .F. ) ;
#2715 = CIRCLE ( 'NONE', #9816, 10.00000000000000888 ) ;
#2717 = CARTESIAN_POINT ( 'NONE',  ( 21.17500000054623044, 26.92701409722686634, 88.54243821818162985 ) ) ;
#2718 = DIRECTION ( 'NONE',  ( 0.000000000000000000, 0.000000000000000000, -1.000000000000000000 ) ) ;
#2719 = LINE ( 'NONE', #6582, #367 ) ;
#2720 = CARTESIAN_POINT ( 'NONE',  ( -1.616912260125061618, 54.74267540711069557, -20.93986429502791324 ) ) ;
#2721 = DIRECTION ( 'NONE',  ( 0.000000000000000000, 0.000000000000000000, 1.000000000000000000 ) ) ;
#2722 = EDGE_CURVE ( 'NONE', #8756, #3198, #70, .T. ) ;
#2723 = CARTESIAN_POINT ( 'NONE',  ( 3.429010155815331973E-15, 45.00000000000000711, 28.00000000000000355 ) ) ;
#2724 = EDGE_LOOP ( 'NONE', ( #11029, #3715, #222, #9925 ) ) ;
#2725 = CARTESIAN_POINT ( 'NONE',  ( -50.00000000000001421, 22.00000000000000000, 188.4007504869563263 ) ) ;
#2726 = CARTESIAN_POINT ( 'NONE',  ( -27.49999999999999645, 20.00000000000000355, 230.4654751958684642 ) ) ;
#2727 = VECTOR ( 'NONE', #6543, 1000.000000000000000 ) ;
#2728 = ADVANCED_FACE ( 'NONE', ( #6854 ), #224, .F. ) ;
#2729 = CARTESIAN_POINT ( 'NONE',  ( 24.57500000054622191, 13.80429023900056684, 86.29171490190961435 ) ) ;
#2730 = CARTESIAN_POINT ( 'NONE',  ( 36.29999999999997584, 13.62011893735970958, 95.42841645007781892 ) ) ;
#2731 = CARTESIAN_POINT ( 'NONE',  ( 37.87500000054622262, 17.63344945572769973, 98.07665518445361386 ) ) ;
#2732 = CARTESIAN_POINT ( 'NONE',  ( 26.07500000054622546, 15.71886984736413417, 96.68563167572563088 ) ) ;
#2733 = CARTESIAN_POINT ( 'NONE',  ( 28.59999999999998721, 12.86707612778636012, 88.47553407664152303 ) ) ;
#2734 = CARTESIAN_POINT ( 'NONE',  ( 34.99999999999999289, 20.00000000000000355, 83.29316153445364534 ) ) ;
#2735 = CARTESIAN_POINT ( 'NONE',  ( 42.67500000054623399, 17.63344945572770328, 83.50966788445364841 ) ) ;
#2736 = VERTEX_POINT ( 'NONE', #11163 ) ;
#2737 = AXIS2_PLACEMENT_3D ( 'NONE', #3284, #10074, #1384 ) ;
#2738 = ADVANCED_FACE ( 'NONE', ( #10094 ), #5211, .F. ) ;
#2739 = CARTESIAN_POINT ( 'NONE',  ( 46.87500000054622262, 22.36655054427230382, 83.50966788445364841 ) ) ;
#2740 = DIRECTION ( 'NONE',  ( -1.000000000000000000, -0.000000000000000000, -0.000000000000000000 ) ) ;
#2741 = VERTEX_POINT ( 'NONE', #11102 ) ;
#2742 = CARTESIAN_POINT ( 'NONE',  ( 4.967426332085672414, 50.65664594515786945, 27.55592256608452573 ) ) ;
#2743 = ORIENTED_EDGE ( 'NONE', *, *, #4161, .T. ) ;
#2744 = DIRECTION ( 'NONE',  ( 0.000000000000000000, 0.000000000000000000, 1.000000000000000000 ) ) ;
#2745 = CARTESIAN_POINT ( 'NONE',  ( 11.99999999999999822, 9.000000000000000000, 0.000000000000000000 ) ) ;
#2746 = CARTESIAN_POINT ( 'NONE',  ( 3.767400715871570327, 46.69623120791406734, -27.74638157013074391 ) ) ;
#2747 = CARTESIAN_POINT ( 'NONE',  ( 42.47500000054623115, 13.07298590277314432, 88.54243821818161564 ) ) ;
#2748 = LINE ( 'NONE', #7442, #7583 ) ;
#2749 = CARTESIAN_POINT ( 'NONE',  ( 48.79999999999999005, 15.59161060780646046, 84.72553407664153724 ) ) ;
#2750 = FACE_OUTER_BOUND ( 'NONE', #157, .T. ) ;
#2751 = CARTESIAN_POINT ( 'NONE',  ( -4.999999999999999112, 49.67330453822126657, 24.49489742783177348 ) ) ;
#2752 = VERTEX_POINT ( 'NONE', #8128 ) ;
#2753 = AXIS2_PLACEMENT_3D ( 'NONE', #11728, #3032, #12487 ) ;
#2754 = CARTESIAN_POINT ( 'NONE',  ( 37.65000000109246514, 20.00000000000000355, 98.29316153445363113 ) ) ;
#2755 = VERTEX_POINT ( 'NONE', #4124 ) ;
#2756 = DIRECTION ( 'NONE',  ( 0.000000000000000000, 0.000000000000000000, -1.000000000000000000 ) ) ;
#2757 = ORIENTED_EDGE ( 'NONE', *, *, #9053, .T. ) ;
#2758 = CARTESIAN_POINT ( 'NONE',  ( -8.673894831530475358, 25.01911591053615425, -23.45021177788830968 ) ) ;
#2759 = DIRECTION ( 'NONE',  ( -0.000000000000000000, -0.000000000000000000, 1.000000000000000000 ) ) ;
#2760 = LINE ( 'NONE', #11331, #10599 ) ;
#2761 = DIRECTION ( 'NONE',  ( -1.000000000000000000, -0.000000000000000000, -0.000000000000000000 ) ) ;
#2762 = LINE ( 'NONE', #736, #1793 ) ;
#2763 = ORIENTED_EDGE ( 'NONE', *, *, #1134, .T. ) ;
#2764 = CARTESIAN_POINT ( 'NONE',  ( 1.136760544875492052, 54.87179675310391502, -27.97737333435675566 ) ) ;
#2765 = DIRECTION ( 'NONE',  ( -0.000000000000000000, -0.000000000000000000, 1.000000000000000000 ) ) ;
#2766 = CARTESIAN_POINT ( 'NONE',  ( 22.17500000054622689, 13.07298590277314254, 93.04388485072563242 ) ) ;
#2767 = ADVANCED_FACE ( 'NONE', ( #11996 ), #10982, .T. ) ;
#2768 = DIRECTION ( 'NONE',  ( 0.000000000000000000, -1.000000000000000000, 0.000000000000000000 ) ) ;
#2769 = CARTESIAN_POINT ( 'NONE',  ( 3.766346521502939471, 53.30452959794249068, -20.66080266315259806 ) ) ;
#2770 = ORIENTED_EDGE ( 'NONE', *, *, #3384, .T. ) ;
#2771 = AXIS2_PLACEMENT_3D ( 'NONE', #8363, #12295, #2649 ) ;
#2772 = LINE ( 'NONE', #2328, #9517 ) ;
#2773 = CARTESIAN_POINT ( 'NONE',  ( -7.307805827056473191, 26.83368120074001695, -19.68893203084326515 ) ) ;
#2774 = DIRECTION ( 'NONE',  ( -1.000000000000000000, -0.000000000000000000, -0.000000000000000000 ) ) ;
#2775 = AXIS2_PLACEMENT_3D ( 'NONE', #10318, #5636, #9383 ) ;
#2776 = CARTESIAN_POINT ( 'NONE',  ( 22.97500000054622760, 24.28113015263587471, 84.90069139318163138 ) ) ;
#2777 = CARTESIAN_POINT ( 'NONE',  ( 6.955575927950914131E-22, 45.00000000000000711, -25.00000000000000000 ) ) ;
#2778 = CARTESIAN_POINT ( 'NONE',  ( -1.298576428593012810, 54.83947011521958359, -20.96226629318544710 ) ) ;
#2779 = CARTESIAN_POINT ( 'NONE',  ( 0.000000000000000000, 70.00000000000000000, -25.00000000000000000 ) ) ;
#2780 = CARTESIAN_POINT ( 'NONE',  ( 26.35000000109246443, 13.62011893735970958, 86.15790661882942914 ) ) ;
#2781 = DIRECTION ( 'NONE',  ( -1.000000000000000000, -0.000000000000000000, -0.000000000000000000 ) ) ;
#2782 = ORIENTED_EDGE ( 'NONE', *, *, #7225, .T. ) ;
#2783 = CARTESIAN_POINT ( 'NONE',  ( 5.000000000000000000, -2.342598717236902051, 4.057500000000004547 ) ) ;
#2784 = EDGE_CURVE ( 'NONE', #136, #1411, #2845, .T. ) ;
#2785 = AXIS2_PLACEMENT_3D ( 'NONE', #9678, #286, #10740 ) ;
#2786 = DIRECTION ( 'NONE',  ( 0.000000000000000000, 0.000000000000000000, -1.000000000000000000 ) ) ;
#2787 = CARTESIAN_POINT ( 'NONE',  ( 28.47500000054622404, 13.07298590277314432, 88.54243821818161564 ) ) ;
#2788 = CARTESIAN_POINT ( 'NONE',  ( 36.09999999999998721, 17.56310227825319004, 98.29316153445361692 ) ) ;
#2789 = CARTESIAN_POINT ( 'NONE',  ( 39.37500000054622973, 26.92701409722686634, 93.04388485072563242 ) ) ;
#2790 = VECTOR ( 'NONE', #6247, 1000.000000000000000 ) ;
#2791 = CARTESIAN_POINT ( 'NONE',  ( 29.57500000054621836, 26.19570976099943493, 95.29460816699764791 ) ) ;
#2792 = CARTESIAN_POINT ( 'NONE',  ( 26.69999999999998508, 13.62011893735971135, 86.15790661882942914 ) ) ;
#2793 = CARTESIAN_POINT ( 'NONE',  ( 30.99999999999998934, 20.00000000000000355, 83.29316153445364534 ) ) ;
#2794 = CARTESIAN_POINT ( 'NONE',  ( 35.07500000054623257, 26.19570976099943493, 86.29171490190961435 ) ) ;
#2795 = VERTEX_POINT ( 'NONE', #267 ) ;
#2796 = CARTESIAN_POINT ( 'NONE',  ( 21.35000000109246443, 26.37988106264029398, 95.42841645007781892 ) ) ;
#2797 = DIRECTION ( 'NONE',  ( -1.000000000000000000, -0.000000000000000000, -0.000000000000000000 ) ) ;
#2798 = VERTEX_POINT ( 'NONE', #9081 ) ;
#2799 = CARTESIAN_POINT ( 'NONE',  ( 8.119414445536275338, 14.15357424190336566, 19.36786064314131650 ) ) ;
#2800 = VERTEX_POINT ( 'NONE', #7041 ) ;
#2801 = CARTESIAN_POINT ( 'NONE',  ( 4.462630933173456604, 28.97330998342967234, -24.60619142875309251 ) ) ;
#2802 = DIRECTION ( 'NONE',  ( 1.000000000000000000, -0.000000000000000000, -0.000000000000000000 ) ) ;
#2803 = CARTESIAN_POINT ( 'NONE',  ( 11.99999999999999645, 0.000000000000000000, 9.000000000000000000 ) ) ;
#2804 = CARTESIAN_POINT ( 'NONE',  ( 41.57500000054622546, 26.19570976099943849, 95.29460816699764791 ) ) ;
#2805 = CARTESIAN_POINT ( 'NONE',  ( 6.000000000000000000, -4.379923479639793449, 2.528750000000004494 ) ) ;
#2806 = ADVANCED_FACE ( 'NONE', ( #329 ), #4313, .F. ) ;
#2807 = SURFACE_STYLE_USAGE ( .BOTH. , #11627 ) ;
#2808 = CARTESIAN_POINT ( 'NONE',  ( 45.87500000054622973, 20.00000000000000355, 98.07665518445361386 ) ) ;
#2809 = CARTESIAN_POINT ( 'NONE',  ( 46.99999999999998579, 20.00000000000000355, 83.29316153445364534 ) ) ;
#2810 = CARTESIAN_POINT ( 'NONE',  ( 8.919948986426568638, 0.000000000000000000, 0.000000000000000000 ) ) ;
#2811 = CARTESIAN_POINT ( 'NONE',  ( 39.05000000109247082, 27.13292387221364876, 88.47553407664153724 ) ) ;
#2812 = AXIS2_PLACEMENT_3D ( 'NONE', #1217, #6030, #3048 ) ;
#2813 = ORIENTED_EDGE ( 'NONE', *, *, #5531, .F. ) ;
#2814 = CARTESIAN_POINT ( 'NONE',  ( 39.75000000109247367, 17.56310227825320425, 98.29316153445363113 ) ) ;
#2815 = CARTESIAN_POINT ( 'NONE',  ( 5.340684424226280325E-17, 55.00000000000000000, -25.00000000000000000 ) ) ;
#2816 = ORIENTED_EDGE ( 'NONE', *, *, #9091, .T. ) ;
#2817 = DIRECTION ( 'NONE',  ( -1.000000000000000000, 0.000000000000000000, 0.000000000000000000 ) ) ;
#2818 = ADVANCED_FACE ( 'NONE', ( #2353 ), #514, .F. ) ;
#2819 = ORIENTED_EDGE ( 'NONE', *, *, #2018, .F. ) ;
#2820 = CARTESIAN_POINT ( 'NONE',  ( -7.533608174404544222, 26.60766787979761006, -23.84262432367340523 ) ) ;
#2821 = CARTESIAN_POINT ( 'NONE',  ( 8.484928971929276642, 14.69808267000900770, -19.21052728408403354 ) ) ;
#2822 = AXIS2_PLACEMENT_3D ( 'NONE', #8251, #5463, #5397 ) ;
#2823 = CARTESIAN_POINT ( 'NONE',  ( -8.123193803314322281, 25.84109844632562769, 23.64424386314666648 ) ) ;
#2824 = VECTOR ( 'NONE', #4395, 999.9999999999998863 ) ;
#2825 = DIRECTION ( 'NONE',  ( 0.000000000000000000, 0.000000000000000000, 1.000000000000000000 ) ) ;
#2826 = CARTESIAN_POINT ( 'NONE',  ( -2.220931175283385350, 45.50830112210639555, 20.88445027029172962 ) ) ;
#2827 = EDGE_LOOP ( 'NONE', ( #6882, #3164, #12009, #4594 ) ) ;
#2828 = CARTESIAN_POINT ( 'NONE',  ( 4.494161248788206997, 52.21552753300132110, -27.63726652259117245 ) ) ;
#2829 = DIRECTION ( 'NONE',  ( 0.000000000000000000, -0.000000000000000000, 1.000000000000000000 ) ) ;
#2830 = CARTESIAN_POINT ( 'NONE',  ( 23.27500000054622120, 27.65831843345427998, 90.79316153445363113 ) ) ;
#2831 = VERTEX_POINT ( 'NONE', #9206 ) ;
#2832 = DIRECTION ( 'NONE',  ( -1.000000000000000000, 0.000000000000000000, 0.000000000000000000 ) ) ;
#2833 = FACE_OUTER_BOUND ( 'NONE', #9349, .T. ) ;
#2834 = ORIENTED_EDGE ( 'NONE', *, *, #7772, .T. ) ;
#2835 = ORIENTED_EDGE ( 'NONE', *, *, #1174, .T. ) ;
#2836 = CARTESIAN_POINT ( 'NONE',  ( 20.99999999999998579, 20.00000000000000355, 83.29316153445364534 ) ) ;
#2837 = EDGE_CURVE ( 'NONE', #4281, #11966, #624, .T. ) ;
#2838 = VECTOR ( 'NONE', #5599, 1000.000000000000000 ) ;
#2839 = PLANE ( 'NONE',  #8451 ) ;
#2840 = CARTESIAN_POINT ( 'NONE',  ( 21.27500000054622475, 27.65831843345427998, 90.79316153445363113 ) ) ;
#2841 = CARTESIAN_POINT ( 'NONE',  ( 0.6521974589784806930, 45.03172573485493047, -24.99359419162020757 ) ) ;
#2842 = DIRECTION ( 'NONE',  ( -1.000000000000000000, -0.000000000000000000, -0.000000000000000000 ) ) ;
#2843 = CARTESIAN_POINT ( 'NONE',  ( 2.217630085887001279, 45.50684883240628409, -20.88476843860882326 ) ) ;
#2844 = EDGE_CURVE ( 'NONE', #7750, #8571, #8843, .T. ) ;
#2845 =( BOUNDED_CURVE ( )  B_SPLINE_CURVE ( 2, ( #451, #5087, #8001, #9147, #7104, #8192, #6160, #1278, #7165, #11873, #11043 ),
 .UNSPECIFIED., .F., .F. ) 
 B_SPLINE_CURVE_WITH_KNOTS ( ( 3, 2, 2, 2, 2, 3 ),
 ( 0.5333333333333333259, 0.5400000000000000355, 0.5466666666666666341, 0.5533333333333333437, 0.5600000000000000533, 0.5666666666666666519 ),
 .UNSPECIFIED. ) 
 CURVE ( )  GEOMETRIC_REPRESENTATION_ITEM ( )  RATIONAL_B_SPLINE_CURVE ( ( 1.000000000000000000, 0.9510565162951535312, 1.000000000000000000, 0.9510565162951535312, 1.000000000000000000, 0.9510565162951535312, 1.000000000000000000, 0.9510565162951535312, 1.000000000000000000, 0.9510565162951535312, 1.000000000000000000 ) ) 
 REPRESENTATION_ITEM ( '' )  );
#2846 = LINE ( 'NONE', #56, #11453 ) ;
#2847 = LINE ( 'NONE', #6709, #6692 ) ;
#2848 = VERTEX_POINT ( 'NONE', #9970 ) ;
#2849 = CARTESIAN_POINT ( 'NONE',  ( 8.654532730718658584, 25.02058024782134282, -23.45477484801500623 ) ) ;
#2850 = EDGE_CURVE ( 'NONE', #2251, #5929, #3240, .T. ) ;
#2851 = CARTESIAN_POINT ( 'NONE',  ( 25.27500000054622475, 26.92701409722686634, 88.54243821818162985 ) ) ;
#2852 = CARTESIAN_POINT ( 'NONE',  ( 48.07500000054622546, 15.71886984736413417, 96.68563167572563088 ) ) ;
#2853 = CARTESIAN_POINT ( 'NONE',  ( 41.57500000054623257, 24.28113015263587116, 96.68563167572563088 ) ) ;
#2854 = CARTESIAN_POINT ( 'NONE',  ( 27.57500000054622191, 26.19570976099943493, 95.29460816699764791 ) ) ;
#2855 = CARTESIAN_POINT ( 'NONE',  ( 32.39999999999998437, 12.86707612778636012, 93.11078899226572503 ) ) ;
#2856 = AXIS2_PLACEMENT_3D ( 'NONE', #3907, #936, #1876 ) ;
#2857 = EDGE_CURVE ( 'NONE', #188, #724, #1346, .T. ) ;
#2858 = CARTESIAN_POINT ( 'NONE',  ( 49.99999999999998579, 40.00000000000000000, 169.9999999999999716 ) ) ;
#2859 = CARTESIAN_POINT ( 'NONE',  ( 31.07500000054622191, 26.19570976099943493, 86.29171490190961435 ) ) ;
#2860 = ORIENTED_EDGE ( 'NONE', *, *, #12102, .F. ) ;
#2861 = CARTESIAN_POINT ( 'NONE',  ( 6.000000000000000000, 2.919948986426538884, 5.057499999999996554 ) ) ;
#2862 = ORIENTED_EDGE ( 'NONE', *, *, #4474, .T. ) ;
#2863 = PRODUCT_RELATED_PRODUCT_CATEGORY ( 'part', '', ( #9041 ) ) ;
#2864 = CARTESIAN_POINT ( 'NONE',  ( -8.656972213103196978, 25.01632711531768294, -26.62861829799461333 ) ) ;
#2865 = ADVANCED_FACE ( 'NONE', ( #7545, #5527 ), #4500, .T. ) ;
#2866 = ORIENTED_EDGE ( 'NONE', *, *, #5273, .F. ) ;
#2867 = CARTESIAN_POINT ( 'NONE',  ( 31.99999999999998579, 20.00000000000000355, 98.29316153445363113 ) ) ;
#2868 = CARTESIAN_POINT ( 'NONE',  ( 8.976146624305494370, 15.54314380353506486, -26.52359378712270299 ) ) ;
#2869 = CARTESIAN_POINT ( 'NONE',  ( 45.87500000054622973, 20.00000000000000355, 98.07665518445361386 ) ) ;
#2870 = CARTESIAN_POINT ( 'NONE',  ( 20.09999999999998721, 17.56310227825320425, 98.29316153445363113 ) ) ;
#2871 = DIRECTION ( 'NONE',  ( -1.000000000000000000, 0.000000000000000000, -0.000000000000000000 ) ) ;
#2872 = CARTESIAN_POINT ( 'NONE',  ( 44.87500000054622973, 20.00000000000000355, 83.50966788445364841 ) ) ;
#2873 = CARTESIAN_POINT ( 'NONE',  ( 45.99999999999998579, 20.00000000000000355, 98.29316153445363113 ) ) ;
#2874 = CARTESIAN_POINT ( 'NONE',  ( 39.89999999999999147, 22.43689772174681707, 98.29316153445361692 ) ) ;
#2875 = CARTESIAN_POINT ( 'NONE',  ( 44.79999999999998295, 15.59161060780646046, 84.72553407664153724 ) ) ;
#2876 = ORIENTED_EDGE ( 'NONE', *, *, #12116, .F. ) ;
#2877 = CARTESIAN_POINT ( 'NONE',  ( 29.15000000109246159, 27.88596668178699645, 90.79316153445363113 ) ) ;
#2878 = DIRECTION ( 'NONE',  ( 0.000000000000000000, 0.000000000000000000, 1.000000000000000000 ) ) ;
#2879 = ORIENTED_EDGE ( 'NONE', *, *, #11416, .F. ) ;
#2880 = LINE ( 'NONE', #790, #2603 ) ;
#2881 = EDGE_CURVE ( 'NONE', #11262, #9504, #2252, .T. ) ;
#2882 = VERTEX_POINT ( 'NONE', #2723 ) ;
#2883 = CARTESIAN_POINT ( 'NONE',  ( -0.6685289520415670372, 30.00000000000001776, -25.00000000000001066 ) ) ;
#2884 = CARTESIAN_POINT ( 'NONE',  ( 9.478226885497544885, 16.74648819031018832, -18.74142151731972561 ) ) ;
#2885 = DIRECTION ( 'NONE',  ( 1.000000000000000000, -0.000000000000000000, -0.000000000000000000 ) ) ;
#2886 = ADVANCED_FACE ( 'NONE', ( #2595 ), #7610, .F. ) ;
#2887 = CARTESIAN_POINT ( 'NONE',  ( 36.97500000054623115, 24.28113015263587471, 84.90069139318163138 ) ) ;
#2888 = CARTESIAN_POINT ( 'NONE',  ( 31.03600000000003689, 0.000000000000000000, 0.000000000000000000 ) ) ;
#2889 = DIRECTION ( 'NONE',  ( 0.000000000000000000, 0.000000000000000000, -1.000000000000000000 ) ) ;
#2890 = CARTESIAN_POINT ( 'NONE',  ( 34.55000000109246372, 17.56310227825320425, 83.29316153445363113 ) ) ;
#2891 = ORIENTED_EDGE ( 'NONE', *, *, #4626, .F. ) ;
#2892 = DIRECTION ( 'NONE',  ( -1.000000000000000000, -0.000000000000000000, -0.000000000000000000 ) ) ;
#2893 = PLANE ( 'NONE',  #2498 ) ;
#2894 = CARTESIAN_POINT ( 'NONE',  ( 48.87500000054622262, 20.00000000000000355, 83.50966788445364841 ) ) ;
#2895 = VERTEX_POINT ( 'NONE', #6585 ) ;
#2896 = DIRECTION ( 'NONE',  ( 0.000000000000000000, 1.000000000000000000, 0.000000000000000000 ) ) ;
#2897 = UNCERTAINTY_MEASURE_WITH_UNIT (LENGTH_MEASURE( 1.000000000000000082E-05 ), #431, 'distance_accuracy_value', 'NONE');
#2898 = CARTESIAN_POINT ( 'NONE',  ( 22.99999999999998934, 20.00000000000000355, 83.29316153445364534 ) ) ;
#2899 = VERTEX_POINT ( 'NONE', #3669 ) ;
#2900 = ORIENTED_EDGE ( 'NONE', *, *, #2322, .F. ) ;
#2901 = AXIS2_PLACEMENT_3D ( 'NONE', #6216, #324, #10089 ) ;
#2902 = DIRECTION ( 'NONE',  ( -1.000000000000000000, 0.000000000000000000, 0.000000000000000000 ) ) ;
#2903 = CARTESIAN_POINT ( 'NONE',  ( -27.49999999999999645, 27.49999999999999645, 145.0000000000000000 ) ) ;
#2904 = CARTESIAN_POINT ( 'NONE',  ( 22.47500000054622760, 13.80429023900056684, 86.29171490190961435 ) ) ;
#2905 = DIRECTION ( 'NONE',  ( 0.000000000000000000, 0.4999999999999983902, -0.8660254037844395958 ) ) ;
#2906 = CIRCLE ( 'NONE', #6153, 25.00000000000000000 ) ;
#2907 = CARTESIAN_POINT ( 'NONE',  ( -3.307603021400832510, 53.76369073917810937, -20.73919124221722043 ) ) ;
#2908 = FACE_OUTER_BOUND ( 'NONE', #3290, .T. ) ;
#2909 = CARTESIAN_POINT ( 'NONE',  ( 26.15000000109246159, 12.11403331821300533, 90.79316153445363113 ) ) ;
#2910 = CARTESIAN_POINT ( 'NONE',  ( 0.000000000000000000, 20.00000000000000355, -70.00000000000000000 ) ) ;
#2911 = VERTEX_POINT ( 'NONE', #1760 ) ;
#2912 = CARTESIAN_POINT ( 'NONE',  ( 37.45000000109246230, 24.40838939219354842, 96.86078899226572503 ) ) ;
#2913 = VECTOR ( 'NONE', #11897, 1000.000000000000000 ) ;
#2914 = CONICAL_SURFACE ( 'NONE', #11634, 5.057500000000000107, 1.047197551196592302 ) ;
#2915 = CARTESIAN_POINT ( 'NONE',  ( 47.57500000054621125, 26.19570976099943493, 95.29460816699764791 ) ) ;
#2916 = CARTESIAN_POINT ( 'NONE',  ( 38.27500000054623541, 12.34168156654572357, 90.79316153445363113 ) ) ;
#2917 =( BOUNDED_CURVE ( )  B_SPLINE_CURVE ( 2, ( #5366, #12150, #8032, #6187, #1311, #3270, #5180, #3390, #359, #7133, #1436 ),
 .UNSPECIFIED., .F., .F. ) 
 B_SPLINE_CURVE_WITH_KNOTS ( ( 3, 2, 2, 2, 2, 3 ),
 ( 0.9000000000000000222, 0.9066666666666666208, 0.9133333333333333304, 0.9200000000000000400, 0.9266666666666666385, 0.9333333333333333481 ),
 .UNSPECIFIED. ) 
 CURVE ( )  GEOMETRIC_REPRESENTATION_ITEM ( )  RATIONAL_B_SPLINE_CURVE ( ( 1.000000000000000000, 0.9510565162951535312, 1.000000000000000000, 0.9510565162951535312, 1.000000000000000000, 0.9510565162951535312, 1.000000000000000000, 0.9510565162951535312, 1.000000000000000000, 0.9510565162951535312, 1.000000000000000000 ) ) 
 REPRESENTATION_ITEM ( '' )  );
#2918 = CARTESIAN_POINT ( 'NONE',  ( 25.07500000054622191, 24.28113015263587471, 84.90069139318163138 ) ) ;
#2919 = CARTESIAN_POINT ( 'NONE',  ( 20.29999999999998650, 13.62011893735971135, 95.42841645007781892 ) ) ;
#2920 = CARTESIAN_POINT ( 'NONE',  ( 30.29999999999998295, 13.62011893735970958, 95.42841645007781892 ) ) ;
#2921 = CARTESIAN_POINT ( 'NONE',  ( 33.47500000054623115, 26.19570976099943493, 95.29460816699764791 ) ) ;
#2922 = VERTEX_POINT ( 'NONE', #6467 ) ;
#2923 = CARTESIAN_POINT ( 'NONE',  ( 6.000000000000000000, 8.759846959279592227, -5.057500000000009877 ) ) ;
#2924 = ORIENTED_EDGE ( 'NONE', *, *, #8828, .T. ) ;
#2925 = EDGE_CURVE ( 'NONE', #7072, #4660, #9518, .T. ) ;
#2926 = CIRCLE ( 'NONE', #2520, 25.50000000000000711 ) ;
#2927 = CARTESIAN_POINT ( 'NONE',  ( 4.680557196582781465, 51.76613573486061171, 27.60609432111097306 ) ) ;
#2928 = VERTEX_POINT ( 'NONE', #4563 ) ;
#2929 =( LENGTH_UNIT ( ) NAMED_UNIT ( * ) SI_UNIT ( .MILLI., .METRE. ) );
#2930 = CARTESIAN_POINT ( 'NONE',  ( 32.29999999999999005, 13.62011893735970958, 95.42841645007781892 ) ) ;
#2931 = CARTESIAN_POINT ( 'NONE',  ( 7.516904306367743871, 13.39678444372546195, -26.97299697137856711 ) ) ;
#2932 = CARTESIAN_POINT ( 'NONE',  ( 44.37500000054622262, 12.34168156654572357, 90.79316153445363113 ) ) ;
#2933 = DIRECTION ( 'NONE',  ( 0.000000000000000000, 0.000000000000000000, -1.000000000000000000 ) ) ;
#2934 = CARTESIAN_POINT ( 'NONE',  ( 42.79999999999999005, 15.59161060780646046, 84.72553407664153724 ) ) ;
#2935 =( GEOMETRIC_REPRESENTATION_CONTEXT ( 3 ) GLOBAL_UNCERTAINTY_ASSIGNED_CONTEXT ( ( #3151 ) ) GLOBAL_UNIT_ASSIGNED_CONTEXT ( ( #10721, #5851, #1905 ) ) REPRESENTATION_CONTEXT ( 'NONE', 'WORKASPACE' ) );
#2936 = CARTESIAN_POINT ( 'NONE',  ( 40.79999999999999005, 15.59161060780646046, 84.72553407664153724 ) ) ;
#2937 = CARTESIAN_POINT ( 'NONE',  ( 0.000000000000000000, 139.9999999999999716, 0.000000000000000000 ) ) ;
#2938 = AXIS2_PLACEMENT_3D ( 'NONE', #851, #1861, #7939 ) ;
#2939 = ORIENTED_EDGE ( 'NONE', *, *, #8320, .T. ) ;
#2940 = CARTESIAN_POINT ( 'NONE',  ( 28.55000000109246372, 17.56310227825321135, 83.29316153445363113 ) ) ;
#2941 = CARTESIAN_POINT ( 'NONE',  ( 4.337692624494786209, 47.49191884430658206, -24.62149689268095187 ) ) ;
#2942 = ORIENTED_EDGE ( 'NONE', *, *, #4970, .F. ) ;
#2943 = VERTEX_POINT ( 'NONE', #4688 ) ;
#2944 = B_SPLINE_CURVE_WITH_KNOTS ( 'NONE', 3,
 ( #5919, #9789, #842, #5673, #9544, #4261, #9092, #6230, #340, #8010, #7115, #4137, #8961, #6043, #275, #213, #7948, #5161, #10990, #11883, #6990, #2299 ),
 .UNSPECIFIED., .F., .F.,
 ( 4, 2, 2, 2, 2, 2, 2, 2, 2, 2, 4 ),
 ( 0.01566371915401241696, 0.01664280665422152028, 0.01762189415443062707, 0.01811143790453518393, 0.01860098165463973732, 0.01958006915484884758, 0.02055915665505796130, 0.02153824415526707156, 0.02202778790537162842, 0.02251733165547618529, 0.02349641915568531983 ),
 .UNSPECIFIED. ) ;
#2945 = FACE_OUTER_BOUND ( 'NONE', #11874, .T. ) ;
#2946 = PRODUCT ( 'socket head cap screw_iso_ISO 4762 M12 x 80 - 36N', 'socket head cap screw_iso_ISO 4762 M12 x 80 - 36N', '', ( #4566 ) ) ;
#2947 = VECTOR ( 'NONE', #1806, 1000.000000000000000 ) ;
#2948 = EDGE_CURVE ( 'NONE', #3442, #4128, #7101, .T. ) ;
#2949 = DIRECTION ( 'NONE',  ( -1.000000000000000000, -0.000000000000000000, -0.000000000000000000 ) ) ;
#2950 = DIRECTION ( 'NONE',  ( 0.000000000000000000, 0.000000000000000000, -1.000000000000000000 ) ) ;
#2951 = CARTESIAN_POINT ( 'NONE',  ( 34.07500000054622546, 13.80429023900056507, 95.29460816699764791 ) ) ;
#2952 = CARTESIAN_POINT ( 'NONE',  ( 39.47500000054622404, 26.92701409722686634, 93.04388485072563242 ) ) ;
#2953 = VECTOR ( 'NONE', #10374, 1000.000000000000000 ) ;
#2954 = CARTESIAN_POINT ( 'NONE',  ( 34.85000000109246798, 24.40838939219355197, 84.72553407664153724 ) ) ;
#2955 = CARTESIAN_POINT ( 'NONE',  ( 43.95000000109245519, 13.62011893735970958, 95.42841645007781892 ) ) ;
#2956 = DIRECTION ( 'NONE',  ( 0.000000000000000000, 0.000000000000000000, 1.000000000000000000 ) ) ;
#2957 = ORIENTED_EDGE ( 'NONE', *, *, #4665, .T. ) ;
#2958 = VECTOR ( 'NONE', #3019, 1000.000000000000000 ) ;
#2959 = DIRECTION ( 'NONE',  ( -1.000000000000000000, 0.000000000000000000, 0.000000000000000000 ) ) ;
#2960 = ORIENTED_EDGE ( 'NONE', *, *, #7602, .T. ) ;
#2961 = CARTESIAN_POINT ( 'NONE',  ( 0.000000000000000000, 0.000000000000000000, 0.000000000000000000 ) ) ;
#2962 = EDGE_LOOP ( 'NONE', ( #6347, #7972, #3483, #9733 ) ) ;
#2963 = EDGE_CURVE ( 'NONE', #949, #10590, #816, .T. ) ;
#2964 = ORIENTED_EDGE ( 'NONE', *, *, #11892, .F. ) ;
#2965 = DIRECTION ( 'NONE',  ( -0.000000000000000000, -0.000000000000000000, 1.000000000000000000 ) ) ;
#2966 =( BOUNDED_CURVE ( )  B_SPLINE_CURVE ( 2, ( #3060, #2102, #5979, #9853, #1168, #8896, #702, #5344, #9340, #1652, #5283, #9399, #12250, #2417, #4570, #8442, #6294, #8199, #3611, #5406, #643, #4506, #12312, #11112, #10275, #6412, #1592, #460, #10165, #5474, #7427, #8382, #7489, #12069, #11230, #11360, #10335, #10103, #3369, #2477, #6352, #9215, #1471, #10220, #581, #3491, #7239, #5534, #521, #11174, #4382, #8259, #4322, #9277, #11297, #4447, #12129, #2602, #8324, #6473, #7299, #3437, #2668, #3553, #1417, #12191, #1533, #7362, #2541, #9154, #5592, #5652, #3734, #10458, #10520, #7741, #889, #11544, #957, #4759, #7616, #3799, #2853, #11479, #5838, #4825, #8625, #4887, #12375, #1833, #6651, #12496, #7679, #5716, #6716, #3865, #3929, #9710, #9463, #3675, #8691, #7553, #1960, #9525, #2789, #761, #5777, #10584, #1, #9583, #6530, #1895, #11676, #9650, #11609, #2916, #11422, #7804, #6780, #2731, #6589, #4632, #64, #10647, #1026, #8748, #1768, #10399, #8502, #1710, #823, #4693, #8566, #12437, #7995, #4052, #11865, #4248, #3043, #3172, #9838, #2982, #4948, #7931, #11795, #8120, #2086, #7035, #4117, #10909, #8060, #2224, #3102, #6847, #2155, #10710, #10976, #2021, #6093, #10841, #383, #5903, #1272, #5206, #9965, #6906, #3234, #5144, #9011, #6027, #7867, #5962, #195, #5013, #9773, #1150, #6972, #10772, #9900, #4185, #1214, #7095, #10028, #1083, #6154, #259, #322, #5080, #2284, #11927, #8948, #1337, #8812, #9075, #131, #3990, #11738, #8877, #565, #2588, #7345, #6460, #12237, #2461, #3418, #3355, #10321, #8184, #7412, #7286, #1638, #11282, #4556, #11216, #6337, #5457, #10205, #11156, #4371, #1516, #4428, #11035, #1579, #5519, #3539, #5393, #9265, #7224, #9386, #12055, #689, #8308, #11990, #3294, #7158, #2527, #12176, #9326, #3479, #6398, #8247, #628, #2345, #6214, #10087, #5266, #10263, #444, #4493, #8367, #1400, #9138, #4306, #11095, #2401, #6278, #10149, #1461, #5329, #9200, #509, #12115, #9448, #5826, #5765, #1697, #5578, #10444, #2776, #1754, #11405, #3663, #7664, #2904, #751, #8613, #4745, #12482, #11349, #8490, #3787, #9511, #11530, #9697, #12362, #2840, #2717, #1884, #6704, #4813, #10385, #2655, #7538, #6580, #4683, #11467, #1819, #4616, #8678, #5638, #811 ),
 .UNSPECIFIED., .F., .F. ) 
 B_SPLINE_CURVE_WITH_KNOTS ( ( 3, 2, 2, 2, 2, 2, 2, 2, 2, 2, 2, 2, 2, 2, 2, 2, 2, 2, 2, 2, 2, 2, 2, 2, 2, 2, 2, 2, 2, 2, 2, 2, 2, 2, 2, 2, 2, 2, 2, 2, 2, 2, 2, 2, 2, 2, 2, 2, 2, 2, 2, 2, 2, 2, 2, 2, 2, 2, 2, 2, 2, 2, 2, 2, 2, 2, 2, 2, 2, 2, 2, 2, 2, 2, 2, 2, 2, 2, 2, 2, 2, 2, 2, 2, 2, 2, 2, 2, 2, 2, 2, 2, 2, 2, 2, 2, 2, 2, 2, 2, 2, 2, 2, 2, 2, 2, 2, 2, 2, 2, 2, 2, 2, 2, 2, 2, 2, 2, 2, 2, 2, 2, 2, 2, 2, 2, 2, 2, 2, 2, 2, 2, 2, 2, 2, 2, 2, 2, 2, 2, 2, 2, 2, 2, 2, 2, 2, 2, 2, 2, 3 ),
 ( 0.000000000000000000, 0.006666666666666667095, 0.01333333333333333419, 0.02000000000000000042, 0.02666666666666666838, 0.03333333333333333287, 0.04000000000000000083, 0.04666666666666666879, 0.05333333333333333676, 0.05999999999999999778, 0.06666666666666666574, 0.07333333333333333370, 0.08000000000000000167, 0.08666666666666666963, 0.09333333333333333759, 0.1000000000000000056, 0.1066666666666666735, 0.1133333333333333276, 0.1199999999999999956, 0.1266666666666666774, 0.1333333333333333315, 0.1400000000000000133, 0.1466666666666666674, 0.1533333333333333215, 0.1600000000000000033, 0.1666666666666666574, 0.1733333333333333393, 0.1799999999999999933, 0.1866666666666666752, 0.1933333333333333293, 0.2000000000000000111, 0.2066666666666666652, 0.2133333333333333470, 0.2200000000000000011, 0.2266666666666666552, 0.2333333333333333370, 0.2399999999999999911, 0.2466666666666666730, 0.2533333333333333548, 0.2600000000000000089, 0.2666666666666666630, 0.2733333333333333171, 0.2800000000000000266, 0.2866666666666666807, 0.2933333333333333348, 0.2999999999999999889, 0.3066666666666666430, 0.3133333333333333526, 0.3200000000000000067, 0.3266666666666666607, 0.3333333333333333148, 0.3400000000000000244, 0.3466666666666666785, 0.3533333333333333326, 0.3599999999999999867, 0.3666666666666666408, 0.3733333333333333504, 0.3800000000000000044, 0.3866666666666666585, 0.3933333333333333126, 0.4000000000000000222, 0.4066666666666666763, 0.4133333333333333304, 0.4199999999999999845, 0.4266666666666666941, 0.4333333333333333481, 0.4400000000000000022, 0.4466666666666666563, 0.4533333333333333104, 0.4600000000000000200, 0.4666666666666666741, 0.4733333333333333282, 0.4799999999999999822, 0.4866666666666666918, 0.4933333333333333459, 0.5000000000000000000, 0.5066666666666667096, 0.5133333333333333082, 0.5200000000000000178, 0.5266666666666666163, 0.5333333333333333259, 0.5400000000000000355, 0.5466666666666666341, 0.5533333333333333437, 0.5600000000000000533, 0.5666666666666666519, 0.5733333333333333615, 0.5799999999999999600, 0.5866666666666666696, 0.5933333333333333792, 0.5999999999999999778, 0.6066666666666666874, 0.6133333333333332860, 0.6199999999999999956, 0.6266666666666667052, 0.6333333333333333037, 0.6400000000000000133, 0.6466666666666666119, 0.6533333333333333215, 0.6600000000000000311, 0.6666666666666666297, 0.6733333333333333393, 0.6800000000000000488, 0.6866666666666666474, 0.6933333333333333570, 0.6999999999999999556, 0.7066666666666666652, 0.7133333333333333748, 0.7199999999999999734, 0.7266666666666666829, 0.7333333333333332815, 0.7399999999999999911, 0.7466666666666667007, 0.7533333333333332993, 0.7600000000000000089, 0.7666666666666667185, 0.7733333333333333171, 0.7800000000000000266, 0.7866666666666666252, 0.7933333333333333348, 0.8000000000000000444, 0.8066666666666666430, 0.8133333333333333526, 0.8199999999999999512, 0.8266666666666666607, 0.8333333333333333703, 0.8399999999999999689, 0.8466666666666666785, 0.8533333333333333881, 0.8599999999999999867, 0.8666666666666666963, 0.8733333333333332948, 0.8800000000000000044, 0.8866666666666667140, 0.8933333333333333126, 0.9000000000000000222, 0.9066666666666666208, 0.9133333333333333304, 0.9200000000000000400, 0.9266666666666666385, 0.9333333333333333481, 0.9399999999999999467, 0.9466666666666666563, 0.9533333333333333659, 0.9599999999999999645, 0.9666666666666666741, 0.9733333333333333837, 0.9799999999999999822, 0.9866666666666666918, 0.9933333333333332904, 1.000000000000000000 ),
 .UNSPECIFIED. ) 
 CURVE ( )  GEOMETRIC_REPRESENTATION_ITEM ( )  RATIONAL_B_SPLINE_CURVE ( ( 1.000000000000000000, 0.9510565162951535312, 1.000000000000000000, 0.9510565162951535312, 1.000000000000000000, 0.9510565162951535312, 1.000000000000000000, 0.9510565162951535312, 1.000000000000000000, 0.9510565162951535312, 1.000000000000000000, 0.9510565162951535312, 1.000000000000000000, 0.9510565162951535312, 1.000000000000000000, 0.9510565162951535312, 1.000000000000000000, 0.9510565162951535312, 1.000000000000000000, 0.9510565162951535312, 1.000000000000000000, 0.9510565162951535312, 1.000000000000000000, 0.9510565162951535312, 1.000000000000000000, 0.9510565162951535312, 1.000000000000000000, 0.9510565162951535312, 1.000000000000000000, 0.9510565162951535312, 1.000000000000000000, 0.9510565162951535312, 1.000000000000000000, 0.9510565162951535312, 1.000000000000000000, 0.9510565162951535312, 1.000000000000000000, 0.9510565162951535312, 1.000000000000000000, 0.9510565162951535312, 1.000000000000000000, 0.9510565162951535312, 1.000000000000000000, 0.9510565162951535312, 1.000000000000000000, 0.9510565162951535312, 1.000000000000000000, 0.9510565162951535312, 1.000000000000000000, 0.9510565162951535312, 1.000000000000000000, 0.9510565162951535312, 1.000000000000000000, 0.9510565162951535312, 1.000000000000000000, 0.9510565162951535312, 1.000000000000000000, 0.9510565162951535312, 1.000000000000000000, 0.9510565162951535312, 1.000000000000000000, 0.9510565162951535312, 1.000000000000000000, 0.9510565162951535312, 1.000000000000000000, 0.9510565162951535312, 1.000000000000000000, 0.9510565162951535312, 1.000000000000000000, 0.9510565162951535312, 1.000000000000000000, 0.9510565162951535312, 1.000000000000000000, 0.9510565162951535312, 1.000000000000000000, 0.9510565162951535312, 1.000000000000000000, 0.9510565162951535312, 1.000000000000000000, 0.9510565162951535312, 1.000000000000000000, 0.9510565162951535312, 1.000000000000000000, 0.9510565162951535312, 1.000000000000000000, 0.9510565162951535312, 1.000000000000000000, 0.9510565162951535312, 1.000000000000000000, 0.9510565162951535312, 1.000000000000000000, 0.9510565162951535312, 1.000000000000000000, 0.9510565162951535312, 1.000000000000000000, 0.9510565162951535312, 1.000000000000000000, 0.9510565162951535312, 1.000000000000000000, 0.9510565162951535312, 1.000000000000000000, 0.9510565162951535312, 1.000000000000000000, 0.9510565162951535312, 1.000000000000000000, 0.9510565162951535312, 1.000000000000000000, 0.9510565162951535312, 1.000000000000000000, 0.9510565162951535312, 1.000000000000000000, 0.9510565162951535312, 1.000000000000000000, 0.9510565162951535312, 1.000000000000000000, 0.9510565162951535312, 1.000000000000000000, 0.9510565162951535312, 1.000000000000000000, 0.9510565162951535312, 1.000000000000000000, 0.9510565162951535312, 1.000000000000000000, 0.9510565162951535312, 1.000000000000000000, 0.9510565162951535312, 1.000000000000000000, 0.9510565162951535312, 1.000000000000000000, 0.9510565162951535312, 1.000000000000000000, 0.9510565162951535312, 1.000000000000000000, 0.9510565162951535312, 1.000000000000000000, 0.9510565162951535312, 1.000000000000000000, 0.9510565162951535312, 1.000000000000000000, 0.9510565162951535312, 1.000000000000000000, 0.9510565162951535312, 1.000000000000000000, 0.9510565162951535312, 1.000000000000000000, 0.9510565162951535312, 1.000000000000000000, 0.9510565162951535312, 1.000000000000000000, 0.9510565162951535312, 1.000000000000000000, 0.9510565162951535312, 1.000000000000000000, 0.9510565162951535312, 1.000000000000000000, 0.9510565162951535312, 1.000000000000000000, 0.9510565162951535312, 1.000000000000000000, 0.9510565162951535312, 1.000000000000000000, 0.9510565162951535312, 1.000000000000000000, 0.9510565162951535312, 1.000000000000000000, 0.9510565162951535312, 1.000000000000000000, 0.9510565162951535312, 1.000000000000000000, 0.9510565162951535312, 1.000000000000000000, 0.9510565162951535312, 1.000000000000000000, 0.9510565162951535312, 1.000000000000000000, 0.9510565162951535312, 1.000000000000000000, 0.9510565162951535312, 1.000000000000000000, 0.9510565162951535312, 1.000000000000000000, 0.9510565162951535312, 1.000000000000000000, 0.9510565162951535312, 1.000000000000000000, 0.9510565162951535312, 1.000000000000000000, 0.9510565162951535312, 1.000000000000000000, 0.9510565162951535312, 1.000000000000000000, 0.9510565162951535312, 1.000000000000000000, 0.9510565162951535312, 1.000000000000000000, 0.9510565162951535312, 1.000000000000000000, 0.9510565162951535312, 1.000000000000000000, 0.9510565162951535312, 1.000000000000000000, 0.9510565162951535312, 1.000000000000000000, 0.9510565162951535312, 1.000000000000000000, 0.9510565162951535312, 1.000000000000000000, 0.9510565162951535312, 1.000000000000000000, 0.9510565162951535312, 1.000000000000000000, 0.9510565162951535312, 1.000000000000000000, 0.9510565162951535312, 1.000000000000000000, 0.9510565162951535312, 1.000000000000000000, 0.9510565162951535312, 1.000000000000000000, 0.9510565162951535312, 1.000000000000000000, 0.9510565162951535312, 1.000000000000000000, 0.9510565162951535312, 1.000000000000000000, 0.9510565162951535312, 1.000000000000000000, 0.9510565162951535312, 1.000000000000000000, 0.9510565162951535312, 1.000000000000000000, 0.9510565162951535312, 1.000000000000000000, 0.9510565162951535312, 1.000000000000000000, 0.9510565162951535312, 1.000000000000000000, 0.9510565162951535312, 1.000000000000000000, 0.9510565162951535312, 1.000000000000000000, 0.9510565162951535312, 1.000000000000000000, 0.9510565162951535312, 1.000000000000000000, 0.9510565162951535312, 1.000000000000000000, 0.9510565162951535312, 1.000000000000000000, 0.9510565162951535312, 1.000000000000000000, 0.9510565162951535312, 1.000000000000000000, 0.9510565162951535312, 1.000000000000000000, 0.9510565162951535312, 1.000000000000000000, 0.9510565162951535312, 1.000000000000000000, 0.9510565162951535312, 1.000000000000000000, 0.9510565162951535312, 1.000000000000000000, 0.9510565162951535312, 1.000000000000000000, 0.9510565162951535312, 1.000000000000000000, 0.9510565162951535312, 1.000000000000000000, 0.9510565162951535312, 1.000000000000000000, 0.9510565162951535312, 1.000000000000000000, 0.9510565162951535312, 1.000000000000000000, 0.9510565162951535312, 1.000000000000000000, 0.9510565162951535312, 1.000000000000000000, 0.9510565162951535312, 1.000000000000000000, 0.9510565162951535312, 1.000000000000000000, 0.9510565162951535312, 1.000000000000000000, 0.9510565162951535312, 1.000000000000000000, 0.9510565162951535312, 1.000000000000000000, 0.9510565162951535312, 1.000000000000000000, 0.9510565162951535312, 1.000000000000000000, 0.9510565162951535312, 1.000000000000000000, 0.9510565162951535312, 1.000000000000000000, 0.9510565162951535312, 1.000000000000000000, 0.9510565162951535312, 1.000000000000000000 ) ) 
 REPRESENTATION_ITEM ( '' )  );
#2967 = CARTESIAN_POINT ( 'NONE',  ( 6.000000000000000000, 5.839897972853064445, -8.673617379884035472E-15 ) ) ;
#2968 = EDGE_CURVE ( 'NONE', #1159, #7590, #7302, .T. ) ;
#2969 = CARTESIAN_POINT ( 'NONE',  ( 7.324799518705101598, 26.80913330496100855, 87.63976656848456059 ) ) ;
#2970 = DIRECTION ( 'NONE',  ( 1.000000000000000000, 0.000000000000000000, 0.000000000000000000 ) ) ;
#2971 = CARTESIAN_POINT ( 'NONE',  ( 6.000000000000000000, 5.839897972853064445, -8.673617379884035472E-15 ) ) ;
#2972 = CARTESIAN_POINT ( 'NONE',  ( -4.838792876751625727, 51.30218438880784504, 20.43503154247634868 ) ) ;
#2973 = VECTOR ( 'NONE', #9723, 1000.000000000000000 ) ;
#2974 = CARTESIAN_POINT ( 'NONE',  ( 26.45000000109246585, 15.59161060780646046, 84.72553407664153724 ) ) ;
#2975 = DIRECTION ( 'NONE',  ( 0.000000000000000000, 0.000000000000000000, 1.000000000000000000 ) ) ;
#2976 = ORIENTED_EDGE ( 'NONE', *, *, #5725, .F. ) ;
#2977 = EDGE_CURVE ( 'NONE', #1932, #1856, #573, .T. ) ;
#2978 = CARTESIAN_POINT ( 'NONE',  ( 37.05000000109246372, 27.13292387221364876, 88.47553407664153724 ) ) ;
#2979 = ITEM_DEFINED_TRANSFORMATION ( 'NONE', 'NONE', #4938,  #9021 ) ;
#2980 = AXIS2_PLACEMENT_3D ( 'NONE', #2135, #5946, #8930 ) ;
#2981 = CARTESIAN_POINT ( 'NONE',  ( 20.37500000054621907, 12.34168156654572357, 90.79316153445363113 ) ) ;
#2982 = CARTESIAN_POINT ( 'NONE',  ( 35.67500000054622689, 22.36655054427230027, 98.07665518445361386 ) ) ;
#2983 = CARTESIAN_POINT ( 'NONE',  ( 23.57500000054622546, 26.19570976099943493, 95.29460816699764791 ) ) ;
#2984 = CARTESIAN_POINT ( 'NONE',  ( 20.49999999999998224, 12.11403331821300533, 90.79316153445363113 ) ) ;
#2985 = CARTESIAN_POINT ( 'NONE',  ( 10.00000000000000355, 20.00000000000000355, -26.15339366124404208 ) ) ;
#2986 = CARTESIAN_POINT ( 'NONE',  ( 32.57500000054623257, 15.71886984736413773, 84.90069139318163138 ) ) ;
#2987 = VERTEX_POINT ( 'NONE', #10450 ) ;
#2988 = DIRECTION ( 'NONE',  ( -1.000000000000000000, 0.000000000000000000, 0.000000000000000000 ) ) ;
#2989 = VERTEX_POINT ( 'NONE', #5399 ) ;
#2990 = LINE ( 'NONE', #10656, #1645 ) ;
#2991 = ORIENTED_EDGE ( 'NONE', *, *, #2079, .F. ) ;
#2992 = LINE ( 'NONE', #9975, #10646 ) ;
#2993 = CARTESIAN_POINT ( 'NONE',  ( 3.239805147987244727, 10.51695055376340804, -27.81856429140262676 ) ) ;
#2994 = CARTESIAN_POINT ( 'NONE',  ( 38.57500000054621836, 13.80429023900056684, 86.29171490190961435 ) ) ;
#2995 = FACE_BOUND ( 'NONE', #450, .T. ) ;
#2996 = EDGE_CURVE ( 'NONE', #5544, #2895, #8559, .T. ) ;
#2997 = CARTESIAN_POINT ( 'NONE',  ( 46.57500000054623257, 13.80429023900056684, 86.29171490190961435 ) ) ;
#2998 = CARTESIAN_POINT ( 'NONE',  ( 41.49999999999997158, 27.88596668178699645, 90.79316153445363113 ) ) ;
#2999 = LINE ( 'NONE', #9792, #886 ) ;
#3000 = CARTESIAN_POINT ( 'NONE',  ( 27.50000000000000355, 27.49999999999999645, 145.0000000000000000 ) ) ;
#3001 = ORIENTED_EDGE ( 'NONE', *, *, #4043, .F. ) ;
#3002 = CARTESIAN_POINT ( 'NONE',  ( 28.85000000109246443, 24.40838939219355197, 84.72553407664153724 ) ) ;
#3003 = CARTESIAN_POINT ( 'NONE',  ( 3.061616998149962604E-15, 10.00000000000000000, 25.00000000000000000 ) ) ;
#3004 = VERTEX_POINT ( 'NONE', #10211 ) ;
#3005 = ORIENTED_EDGE ( 'NONE', *, *, #10572, .T. ) ;
#3006 = CARTESIAN_POINT ( 'NONE',  ( -4.461205683540790723, 28.97367431253432812, -24.60633856694852994 ) ) ;
#3007 = CARTESIAN_POINT ( 'NONE',  ( 0.6000000000000033085, 0.000000000000000000, 9.000000000000000000 ) ) ;
#3008 = LINE ( 'NONE', #9931, #4736 ) ;
#3009 = CIRCLE ( 'NONE', #4423, 7.500000000000000000 ) ;
#3010 = CARTESIAN_POINT ( 'NONE',  ( 38.27500000054623541, 12.34168156654572535, 90.79316153445363113 ) ) ;
#3011 = CARTESIAN_POINT ( 'NONE',  ( 30.97500000054622760, 22.36655054427230382, 83.50966788445364841 ) ) ;
#3012 = DIRECTION ( 'NONE',  ( 0.000000000000000000, 0.000000000000000000, 1.000000000000000000 ) ) ;
#3013 = CARTESIAN_POINT ( 'NONE',  ( 43.65000000109246514, 20.00000000000000355, 98.29316153445363113 ) ) ;
#3014 = DIRECTION ( 'NONE',  ( 0.000000000000000000, 0.000000000000000000, 1.000000000000000000 ) ) ;
#3015 = ORIENTED_EDGE ( 'NONE', *, *, #5634, .T. ) ;
#3016 = EDGE_CURVE ( 'NONE', #3699, #9751, #12185, .T. ) ;
#3017 = CARTESIAN_POINT ( 'NONE',  ( 3.307338549894080604, 53.76391169785250668, -24.78134996739077422 ) ) ;
#3018 = ORIENTED_EDGE ( 'NONE', *, *, #9369, .T. ) ;
#3019 = DIRECTION ( 'NONE',  ( 0.000000000000000000, 1.000000000000000000, -1.039664082171044875E-15 ) ) ;
#3020 = ORIENTED_EDGE ( 'NONE', *, *, #11242, .F. ) ;
#3021 = AXIS2_PLACEMENT_3D ( 'NONE', #3237, #1154, #9776 ) ;
#3022 = PRODUCT_RELATED_PRODUCT_CATEGORY ( 'part', '', ( #2946 ) ) ;
#3023 =( REPRESENTATION_RELATIONSHIP ('NONE','NONE', #4262, #4339 ) REPRESENTATION_RELATIONSHIP_WITH_TRANSFORMATION ( #2979 )SHAPE_REPRESENTATION_RELATIONSHIP( ) );
#3024 = ORIENTED_EDGE ( 'NONE', *, *, #8314, .F. ) ;
#3025 = EDGE_CURVE ( 'NONE', #7179, #481, #818, .T. ) ;
#3026 = TOROIDAL_SURFACE ( 'NONE', #6652, 17.49999999999996803, 10.00000000000000000 ) ;
#3027 = CYLINDRICAL_SURFACE ( 'NONE', #1950, 5.000000000000000000 ) ;
#3028 = CARTESIAN_POINT ( 'NONE',  ( 0.000000000000000000, 0.000000000000000000, -25.00000000000000000 ) ) ;
#3029 = DIRECTION ( 'NONE',  ( -0.7071067811865342501, 0.000000000000000000, 0.7071067811865608954 ) ) ;
#3030 = CARTESIAN_POINT ( 'NONE',  ( 4.462445293788150025, 28.95508627606223229, 20.52252167446830100 ) ) ;
#3031 = CARTESIAN_POINT ( 'NONE',  ( 3.061617023331388775E-15, 45.00000000000000711, 25.00000000000000000 ) ) ;
#3032 = DIRECTION ( 'NONE',  ( 0.000000000000000000, 0.000000000000000000, 1.000000000000000000 ) ) ;
#3033 = CARTESIAN_POINT ( 'NONE',  ( 41.47500000054623115, 26.19570976099943493, 95.29460816699764791 ) ) ;
#3034 = PLANE ( 'NONE',  #5887 ) ;
#3035 = ORIENTED_EDGE ( 'NONE', *, *, #7930, .F. ) ;
#3036 = CARTESIAN_POINT ( 'NONE',  ( -3.709758735690515970E-18, 30.00000000000001066, -25.00000000000000000 ) ) ;
#3037 = EDGE_CURVE ( 'NONE', #2485, #2795, #3484, .T. ) ;
#3038 = PRODUCT_CONTEXT ( 'NONE', #1566, 'mechanical' ) ;
#3039 =( BOUNDED_CURVE ( )  B_SPLINE_CURVE ( 2, ( #4433, #10389, #512, #3602, #3482, #9141, #12181, #12058, #7350, #3359, #11221 ),
 .UNSPECIFIED., .F., .F. ) 
 B_SPLINE_CURVE_WITH_KNOTS ( ( 3, 2, 2, 2, 2, 3 ),
 ( 0.4666666666666666186, 0.4733333333333332726, 0.4799999999999999267, 0.4866666666666666918, 0.4933333333333333459, 0.5000000000000000000 ),
 .UNSPECIFIED. ) 
 CURVE ( )  GEOMETRIC_REPRESENTATION_ITEM ( )  RATIONAL_B_SPLINE_CURVE ( ( 1.000000000000000444, 0.9510565162951531981, 1.000000000000000000, 0.9510565162951535312, 1.000000000000000000, 0.9510565162951535312, 1.000000000000000000, 0.9510565162951535312, 1.000000000000000000, 0.9510565162951535312, 1.000000000000000000 ) ) 
 REPRESENTATION_ITEM ( '' )  );
#3040 = CARTESIAN_POINT ( 'NONE',  ( 20.27500000054622475, 13.07298590277314254, 93.04388485072563242 ) ) ;
#3041 = CARTESIAN_POINT ( 'NONE',  ( 24.65000000109246514, 20.00000000000000355, 83.29316153445364534 ) ) ;
#3042 = EDGE_CURVE ( 'NONE', #2279, #12065, #11152, .T. ) ;
#3043 = CARTESIAN_POINT ( 'NONE',  ( 35.97500000054623115, 15.71886984736413417, 96.68563167572563088 ) ) ;
#3044 = EDGE_CURVE ( 'NONE', #8530, #1878, #4880, .T. ) ;
#3045 = EDGE_CURVE ( 'NONE', #11194, #1279, #7509, .T. ) ;
#3046 = CARTESIAN_POINT ( 'NONE',  ( 23.87500000054622262, 20.00000000000000355, 98.07665518445361386 ) ) ;
#3047 = CARTESIAN_POINT ( 'NONE',  ( 24.29999999999999005, 13.62011893735971135, 95.42841645007781892 ) ) ;
#3048 = DIRECTION ( 'NONE',  ( 0.000000000000000000, 0.000000000000000000, -1.000000000000000000 ) ) ;
#3049 = CARTESIAN_POINT ( 'NONE',  ( 34.67500000054621268, 17.63344945572770328, 83.50966788445364841 ) ) ;
#3050 = ORIENTED_EDGE ( 'NONE', *, *, #3042, .T. ) ;
#3051 = DIRECTION ( 'NONE',  ( 0.000000000000000000, 0.000000000000000000, 1.000000000000000000 ) ) ;
#3052 = VERTEX_POINT ( 'NONE', #6899 ) ;
#3053 = CARTESIAN_POINT ( 'NONE',  ( 2.505714055585114508, 54.33929830399747374, 27.88900956191349678 ) ) ;
#3054 = ORIENTED_EDGE ( 'NONE', *, *, #11635, .F. ) ;
#3055 = CARTESIAN_POINT ( 'NONE',  ( -50.00000000000001421, 22.00000000000000000, 188.4007504869563263 ) ) ;
#3056 = CYLINDRICAL_SURFACE ( 'NONE', #8069, 7.499999999999992895 ) ;
#3057 = VECTOR ( 'NONE', #11045, 1000.000000000000000 ) ;
#3058 = CARTESIAN_POINT ( 'NONE',  ( 35.67500000054622689, 24.28113015263587116, 96.68563167572563088 ) ) ;
#3059 = DIRECTION ( 'NONE',  ( -1.000000000000000000, -0.000000000000000000, -0.000000000000000000 ) ) ;
#3060 = CARTESIAN_POINT ( 'NONE',  ( 49.77500000054622831, 20.00000000000000355, 98.07665518445361386 ) ) ;
#3061 = CARTESIAN_POINT ( 'NONE',  ( 41.67500000054622689, 24.28113015263587116, 96.68563167572563088 ) ) ;
#3062 = CARTESIAN_POINT ( 'NONE',  ( 40.79999999999999005, 15.59161060780646046, 84.72553407664153724 ) ) ;
#3063 = CARTESIAN_POINT ( 'NONE',  ( 39.79999999999999005, 24.40838939219354842, 96.86078899226572503 ) ) ;
#3064 = FACE_OUTER_BOUND ( 'NONE', #8000, .T. ) ;
#3065 = ORIENTED_EDGE ( 'NONE', *, *, #6049, .F. ) ;
#3066 = CARTESIAN_POINT ( 'NONE',  ( 33.15000000109246514, 27.88596668178699645, 90.79316153445363113 ) ) ;
#3067 = CARTESIAN_POINT ( 'NONE',  ( 2.644456282953588921, 45.75339465611970269, -24.86012065554512063 ) ) ;
#3068 = ORIENTED_EDGE ( 'NONE', *, *, #7234, .F. ) ;
#3069 = ORIENTED_EDGE ( 'NONE', *, *, #10523, .T. ) ;
#3070 = CARTESIAN_POINT ( 'NONE',  ( 27.49999999999999645, 20.00000000000000355, 197.9999999999999716 ) ) ;
#3071 = CARTESIAN_POINT ( 'NONE',  ( -4.968205859249467338, 50.65222807605660904, -24.50145347565533882 ) ) ;
#3072 = FACE_OUTER_BOUND ( 'NONE', #3256, .T. ) ;
#3073 = CARTESIAN_POINT ( 'NONE',  ( 31.77500000054622831, 20.00000000000000355, 98.07665518445361386 ) ) ;
#3074 = CARTESIAN_POINT ( 'NONE',  ( 29.37500000054622618, 27.65831843345427998, 90.79316153445363113 ) ) ;
#3075 = CARTESIAN_POINT ( 'NONE',  ( 44.35000000109246798, 13.62011893735970958, 86.15790661882942914 ) ) ;
#3076 = DIRECTION ( 'NONE',  ( -1.000000000000000000, 0.000000000000000000, 0.000000000000000000 ) ) ;
#3077 = ORIENTED_EDGE ( 'NONE', *, *, #8511, .F. ) ;
#3078 = CARTESIAN_POINT ( 'NONE',  ( 49.27500000054622120, 26.92701409722686634, 88.54243821818162985 ) ) ;
#3079 = CARTESIAN_POINT ( 'NONE',  ( 47.25000000109246656, 27.13292387221364876, 93.11078899226573924 ) ) ;
#3080 = ORIENTED_EDGE ( 'NONE', *, *, #1693, .T. ) ;
#3081 = CARTESIAN_POINT ( 'NONE',  ( 19.65000000109246514, 20.00000000000000355, 98.29316153445363113 ) ) ;
#3082 = ORIENTED_EDGE ( 'NONE', *, *, #12202, .F. ) ;
#3083 = EDGE_CURVE ( 'NONE', #2354, #5181, #8805, .T. ) ;
#3084 = CARTESIAN_POINT ( 'NONE',  ( -6.999999999999999112, 40.00000000000000000, 132.8533255156884820 ) ) ;
#3085 = DIRECTION ( 'NONE',  ( 0.7071067811865502373, 0.000000000000000000, 0.7071067811865449082 ) ) ;
#3086 = CYLINDRICAL_SURFACE ( 'NONE', #11276, 5.000000000000000888 ) ;
#3087 = DIRECTION ( 'NONE',  ( 0.000000000000000000, 0.000000000000000000, -1.000000000000000000 ) ) ;
#3088 = CARTESIAN_POINT ( 'NONE',  ( 7.147088427834759727, 26.99542114996404507, 93.50820798009134194 ) ) ;
#3089 = CARTESIAN_POINT ( 'NONE',  ( 4.743618752923510762, 48.38567045510036735, -24.54617134760821173 ) ) ;
#3090 = CARTESIAN_POINT ( 'NONE',  ( 27.49999999999999645, 20.00000000000000355, 189.9999999999999716 ) ) ;
#3091 = CARTESIAN_POINT ( 'NONE',  ( -0.8195736974120422236, 54.93507064933334050, 20.98461236856086032 ) ) ;
#3092 = DIRECTION ( 'NONE',  ( -0.000000000000000000, -0.000000000000000000, -1.000000000000000000 ) ) ;
#3093 = CARTESIAN_POINT ( 'NONE',  ( 43.47500000054623115, 26.19570976099943493, 95.29460816699764791 ) ) ;
#3094 = AXIS2_PLACEMENT_3D ( 'NONE', #12494, #3798, #3610 ) ;
#3095 = CARTESIAN_POINT ( 'NONE',  ( -20.00000000000000355, 24.39339828220178674, 137.5000000000000000 ) ) ;
#3096 = ORIENTED_EDGE ( 'NONE', *, *, #1774, .T. ) ;
#3097 = CARTESIAN_POINT ( 'NONE',  ( -4.444287400701609769, 11.03583284713306689, -27.64660125085886122 ) ) ;
#3098 = EDGE_CURVE ( 'NONE', #10212, #3211, #4046, .T. ) ;
#3099 = EDGE_CURVE ( 'NONE', #5557, #9486, #2641, .T. ) ;
#3100 = CARTESIAN_POINT ( 'NONE',  ( 13.64110105645934290, 20.00000000000000355, 187.9999999999999716 ) ) ;
#3101 = VECTOR ( 'NONE', #1629, 1000.000000000000000 ) ;
#3102 = CARTESIAN_POINT ( 'NONE',  ( 34.57500000054623257, 15.71886984736413773, 84.90069139318163138 ) ) ;
#3103 = CARTESIAN_POINT ( 'NONE',  ( 21.37500000054622262, 27.65831843345427998, 90.79316153445363113 ) ) ;
#3104 = CARTESIAN_POINT ( 'NONE',  ( 24.19999999999998863, 15.59161060780645691, 96.86078899226572503 ) ) ;
#3105 = ADVANCED_FACE ( 'NONE', ( #57 ), #4878, .T. ) ;
#3106 = CARTESIAN_POINT ( 'NONE',  ( -50.00000000000001421, 92.00000000000000000, 166.8533255156881694 ) ) ;
#3107 = CARTESIAN_POINT ( 'NONE',  ( 25.07500000054623257, 26.19570976099943493, 86.29171490190961435 ) ) ;
#3108 = ORIENTED_EDGE ( 'NONE', *, *, #6601, .T. ) ;
#3109 = CARTESIAN_POINT ( 'NONE',  ( 6.000000000000000000, -5.839897972853060892, 7.806255641895631925E-15 ) ) ;
#3110 = FACE_OUTER_BOUND ( 'NONE', #5693, .T. ) ;
#3111 = VERTEX_POINT ( 'NONE', #4133 ) ;
#3112 = CARTESIAN_POINT ( 'NONE',  ( 4.492035651432232157, 52.22013966317427247, 27.63761663118750533 ) ) ;
#3113 = ORIENTED_EDGE ( 'NONE', *, *, #6355, .T. ) ;
#3114 = CIRCLE ( 'NONE', #4537, 7.499999999999992895 ) ;
#3115 = ADVANCED_FACE ( 'NONE', ( #3920 ), #3034, .F. ) ;
#3116 = CARTESIAN_POINT ( 'NONE',  ( 3.429010155815331973E-15, 45.00000000000000711, 28.00000000000000355 ) ) ;
#3117 = PRODUCT_DEFINITION_FORMATION_WITH_SPECIFIED_SOURCE ( 'ANY', '', #9041, .NOT_KNOWN. ) ;
#3118 = LINE ( 'NONE', #1164, #8438 ) ;
#3119 = CARTESIAN_POINT ( 'NONE',  ( 40.25000000109246656, 12.86707612778636012, 88.47553407664152303 ) ) ;
#3120 = CARTESIAN_POINT ( 'NONE',  ( 26.89999999999998792, 17.56310227825324333, 83.29316153445360271 ) ) ;
#3121 = CARTESIAN_POINT ( 'NONE',  ( 40.47500000054622404, 13.07298590277314432, 88.54243821818161564 ) ) ;
#3122 = CARTESIAN_POINT ( 'NONE',  ( 40.29999999999997584, 13.62011893735971135, 95.42841645007781892 ) ) ;
#3123 = EDGE_CURVE ( 'NONE', #6417, #2265, #4670, .T. ) ;
#3124 = CARTESIAN_POINT ( 'NONE',  ( 0.000000000000000000, 20.00000000000000355, 69.99999999999998579 ) ) ;
#3125 = CARTESIAN_POINT ( 'NONE',  ( 5.000000000000000000, 4.685197434473814759, -5.637851296924623057E-15 ) ) ;
#3126 = ORIENTED_EDGE ( 'NONE', *, *, #8777, .F. ) ;
#3127 = VECTOR ( 'NONE', #3327, 1000.000000000000000 ) ;
#3128 = CARTESIAN_POINT ( 'NONE',  ( 31.25000000109246656, 27.13292387221364876, 93.11078899226573924 ) ) ;
#3129 = CARTESIAN_POINT ( 'NONE',  ( 3.975724277407679974, 46.95046481276702366, -24.68253032026751370 ) ) ;
#3130 = ORIENTED_EDGE ( 'NONE', *, *, #6068, .T. ) ;
#3131 = FACE_OUTER_BOUND ( 'NONE', #7454, .T. ) ;
#3132 = ORIENTED_EDGE ( 'NONE', *, *, #3083, .F. ) ;
#3133 = CARTESIAN_POINT ( 'NONE',  ( 91.03600000000000136, 0.000000000000000000, 5.999999999999998224 ) ) ;
#3134 = FACE_OUTER_BOUND ( 'NONE', #9033, .T. ) ;
#3135 = VECTOR ( 'NONE', #5382, 999.9999999999998863 ) ;
#3136 = DIRECTION ( 'NONE',  ( 0.000000000000000000, 0.000000000000000000, -1.000000000000000000 ) ) ;
#3137 = CARTESIAN_POINT ( 'NONE',  ( 31.07500000054622191, 26.19570976099943493, 86.29171490190961435 ) ) ;
#3138 = CARTESIAN_POINT ( 'NONE',  ( 29.77500000054622120, 22.36655054427230027, 98.07665518445361386 ) ) ;
#3139 = CARTESIAN_POINT ( 'NONE',  ( -4.839010323211785369, 51.30044682260506761, 27.57876396239285555 ) ) ;
#3140 = CARTESIAN_POINT ( 'NONE',  ( 4.455554066248277323, 28.97648380245139066, -27.64996667850891754 ) ) ;
#3141 = CARTESIAN_POINT ( 'NONE',  ( 33.95000000109246940, 13.62011893735970958, 95.42841645007781892 ) ) ;
#3142 = ORIENTED_EDGE ( 'NONE', *, *, #12274, .T. ) ;
#3143 = CARTESIAN_POINT ( 'NONE',  ( 27.49999999999999645, 20.00000000000000355, 172.0000000000000000 ) ) ;
#3144 = ORIENTED_EDGE ( 'NONE', *, *, #8073, .F. ) ;
#3145 = CARTESIAN_POINT ( 'NONE',  ( -34.99999999999997868, 20.00000000000000000, 137.5000000000000000 ) ) ;
#3146 = AXIS2_PLACEMENT_3D ( 'NONE', #7576, #3852, #1946 ) ;
#3147 = EDGE_LOOP ( 'NONE', ( #3216, #9096, #11161, #7060 ) ) ;
#3148 = TOROIDAL_SURFACE ( 'NONE', #4152, 6.599999999999999645, 0.5999999999999999778 ) ;
#3149 = LINE ( 'NONE', #1131, #3937 ) ;
#3150 = CARTESIAN_POINT ( 'NONE',  ( -8.118656623617184209, 14.15260872815194126, -19.36816941975095574 ) ) ;
#3151 = UNCERTAINTY_MEASURE_WITH_UNIT (LENGTH_MEASURE( 1.000000000000000082E-05 ), #10721, 'distance_accuracy_value', 'NONE');
#3152 = CARTESIAN_POINT ( 'NONE',  ( 0.000000000000000000, 139.9999999999999716, 0.000000000000000000 ) ) ;
#3153 = CONICAL_SURFACE ( 'NONE', #3358, 5.035999999999999588, 0.7853981633974671528 ) ;
#3154 = FACE_OUTER_BOUND ( 'NONE', #9605, .T. ) ;
#3155 = PRODUCT_DEFINITION_SHAPE ( 'NONE', 'NONE',  #12554 ) ;
#3156 = CARTESIAN_POINT ( 'NONE',  ( 6.689122664262947993, 27.43351973878651862, 91.82200081781293477 ) ) ;
#3157 = EDGE_CURVE ( 'NONE', #7779, #6828, #5956, .T. ) ;
#3158 = CARTESIAN_POINT ( 'NONE',  ( 3.303834617765012194, 46.23291288788979614, -24.78182658752202983 ) ) ;
#3159 = CARTESIAN_POINT ( 'NONE',  ( -1.612729787338046394, 45.25594143338945941, -24.94976830077123964 ) ) ;
#3160 = CARTESIAN_POINT ( 'NONE',  ( -3.767196188295967918, 53.30371400289418915, 20.66066053404689029 ) ) ;
#3161 = CARTESIAN_POINT ( 'NONE',  ( -6.999999999999999112, 84.49999999999998579, 101.8533255156881978 ) ) ;
#3162 = CARTESIAN_POINT ( 'NONE',  ( 44.37500000054622973, 13.07298590277314432, 88.54243821818161564 ) ) ;
#3163 = CARTESIAN_POINT ( 'NONE',  ( -23.10660171779820971, 27.49999999999999645, 140.6066017177982133 ) ) ;
#3164 = ORIENTED_EDGE ( 'NONE', *, *, #5095, .T. ) ;
#3165 = ADVANCED_FACE ( 'NONE', ( #7923 ), #5771, .F. ) ;
#3166 = B_SPLINE_CURVE_WITH_KNOTS ( 'NONE', 3,
 ( #11982, #6085, #1389, #3288, #6018, #7149, #3225, #1204, #10900, #5071, #8937, #8051, #436, #250, #4106, #6143, #10018, #1326, #11025, #5197, #2337, #6206 ),
 .UNSPECIFIED., .F., .F.,
 ( 4, 2, 2, 2, 2, 2, 2, 2, 2, 2, 4 ),
 ( 0.01566368669230110838, 0.01664276945100601549, 0.01762185220971091912, 0.01811139358906338134, 0.01860093496841584357, 0.01958001772712077149, 0.02055910048582569594, 0.02153818324453062039, 0.02202772462388308261, 0.02251726600323554484, 0.02349634876194046582 ),
 .UNSPECIFIED. ) ;
#3167 = CARTESIAN_POINT ( 'NONE',  ( -4.331872009808981794, 52.50234731214368367, 24.62196273622729592 ) ) ;
#3168 = AXIS2_PLACEMENT_3D ( 'NONE', #3277, #4032, #10889 ) ;
#3169 = CARTESIAN_POINT ( 'NONE',  ( 21.47500000054622404, 26.92701409722686634, 93.04388485072563242 ) ) ;
#3170 = CARTESIAN_POINT ( 'NONE',  ( 42.67500000054622689, 15.71886984736413773, 84.90069139318163138 ) ) ;
#3171 = VECTOR ( 'NONE', #1255, 1000.000000000000000 ) ;
#3172 = CARTESIAN_POINT ( 'NONE',  ( 35.87500000054622262, 17.63344945572769973, 98.07665518445361386 ) ) ;
#3173 = CARTESIAN_POINT ( 'NONE',  ( 21.17500000054622689, 26.19570976099943493, 86.29171490190961435 ) ) ;
#3174 = CARTESIAN_POINT ( 'NONE',  ( 21.89999999999999147, 22.43689772174679575, 98.29316153445363113 ) ) ;
#3175 = FACE_OUTER_BOUND ( 'NONE', #12522, .T. ) ;
#3176 = CARTESIAN_POINT ( 'NONE',  ( 28.17500000054622689, 13.07298590277314254, 93.04388485072563242 ) ) ;
#3177 = ORIENTED_EDGE ( 'NONE', *, *, #2508, .T. ) ;
#3178 = B_SPLINE_CURVE_WITH_KNOTS ( 'NONE', 3,
 ( #2509, #3464, #6561, #5501, #8288, #7520, #5560, #5374, #1678, #9370, #9245, #610, #12158, #11199, #7391, #10426, #11139, #1498, #3581, #670, #548, #4536, #6500, #4600, #7328, #3641 ),
 .UNSPECIFIED., .F., .F.,
 ( 4, 2, 2, 2, 2, 2, 2, 2, 2, 2, 2, 2, 4 ),
 ( 0.01580552869034228605, 0.01679261472842853362, 0.01777970076651477771, 0.01975387284268728671, 0.02172804491885978878, 0.02271513095694604328, 0.02370221699503229779, 0.02567638907120481373, 0.02666347510929107170, 0.02765056114737732967, 0.02962473322354984562, 0.03061181926163610706, 0.03159890529972236156 ),
 .UNSPECIFIED. ) ;
#3179 = EDGE_CURVE ( 'NONE', #1799, #3939, #9343, .T. ) ;
#3180 = CARTESIAN_POINT ( 'NONE',  ( 23.15000000109246514, 27.88596668178699645, 90.79316153445363113 ) ) ;
#3181 = ORIENTED_EDGE ( 'NONE', *, *, #4811, .F. ) ;
#3182 = ORIENTED_EDGE ( 'NONE', *, *, #7196, .T. ) ;
#3183 = LINE ( 'NONE', #3874, #5294 ) ;
#3184 = ORIENTED_EDGE ( 'NONE', *, *, #8798, .F. ) ;
#3185 = CYLINDRICAL_SURFACE ( 'NONE', #325, 10.00000000000000355 ) ;
#3186 = EDGE_CURVE ( 'NONE', #3442, #9941, #4752, .T. ) ;
#3187 = CARTESIAN_POINT ( 'NONE',  ( 40.55000000109246372, 17.56310227825320425, 83.29316153445363113 ) ) ;
#3188 = DIRECTION ( 'NONE',  ( -1.000000000000000000, -0.000000000000000000, -0.000000000000000000 ) ) ;
#3189 = CARTESIAN_POINT ( 'NONE',  ( 39.97500000054623115, 17.63344945572769973, 98.07665518445361386 ) ) ;
#3190 = CARTESIAN_POINT ( 'NONE',  ( 45.19999999999998863, 24.40838939219355197, 84.72553407664153724 ) ) ;
#3191 = CONICAL_SURFACE ( 'NONE', #4608, 5.035999999999999588, 0.7853981633974514986 ) ;
#3192 = CARTESIAN_POINT ( 'NONE',  ( 48.67500000054623399, 17.63344945572770328, 83.50966788445364841 ) ) ;
#3193 = ORIENTED_EDGE ( 'NONE', *, *, #11210, .F. ) ;
#3194 = CARTESIAN_POINT ( 'NONE',  ( 24.65000000109246514, 20.00000000000000355, 83.29316153445364534 ) ) ;
#3195 = CARTESIAN_POINT ( 'NONE',  ( -50.00000000000001421, 40.00000000000000000, 69.99999999999998579 ) ) ;
#3196 = ORIENTED_EDGE ( 'NONE', *, *, #11378, .F. ) ;
#3197 = CARTESIAN_POINT ( 'NONE',  ( 23.19999999999998863, 24.40838939219355197, 84.72553407664153724 ) ) ;
#3198 = VERTEX_POINT ( 'NONE', #12488 ) ;
#3199 = CARTESIAN_POINT ( 'NONE',  ( 7.950351283875114028, 13.89977645389732253, 26.85022583157104137 ) ) ;
#3200 = EDGE_CURVE ( 'NONE', #10184, #4281, #3793, .T. ) ;
#3201 = CIRCLE ( 'NONE', #12514, 25.49999999999998934 ) ;
#3202 = DIRECTION ( 'NONE',  ( -0.000000000000000000, -0.000000000000000000, 1.000000000000000000 ) ) ;
#3203 = PRODUCT_DEFINITION_CONTEXT ( 'detailed design', #9995, 'design' ) ;
#3204 = CARTESIAN_POINT ( 'NONE',  ( 27.77500000054622831, 20.00000000000000355, 98.07665518445361386 ) ) ;
#3205 = CARTESIAN_POINT ( 'NONE',  ( 34.17500000054622689, 13.80429023900056507, 95.29460816699764791 ) ) ;
#3206 = CARTESIAN_POINT ( 'NONE',  ( -50.00000000000001421, 92.00000000000000000, 69.99999999999998579 ) ) ;
#3207 = EDGE_CURVE ( 'NONE', #8345, #1560, #2847, .T. ) ;
#3208 = CARTESIAN_POINT ( 'NONE',  ( 7.519126441075570710, 26.60062706338189642, 23.84344315696457173 ) ) ;
#3209 = CARTESIAN_POINT ( 'NONE',  ( -0.3269774092232215490, 45.00000000000000000, 25.00000000000000711 ) ) ;
#3210 = VECTOR ( 'NONE', #2501, 1000.000000000000000 ) ;
#3211 = VERTEX_POINT ( 'NONE', #4300 ) ;
#3212 = DIRECTION ( 'NONE',  ( -1.000000000000000000, 0.000000000000000000, 0.000000000000000000 ) ) ;
#3213 = DIRECTION ( 'NONE',  ( 0.000000000000000000, 0.000000000000000000, -1.000000000000000000 ) ) ;
#3214 = ORIENTED_EDGE ( 'NONE', *, *, #5340, .F. ) ;
#3215 = CARTESIAN_POINT ( 'NONE',  ( -6.500000000000214051, 0.000000000000000000, 26.49999999999998934 ) ) ;
#3216 = ORIENTED_EDGE ( 'NONE', *, *, #8359, .F. ) ;
#3217 = CARTESIAN_POINT ( 'NONE',  ( -6.110563603929655585, 12.05744620208248286, -24.24805373538051967 ) ) ;
#3218 = AXIS2_PLACEMENT_3D ( 'NONE', #5318, #9314, #373 ) ;
#3219 = CARTESIAN_POINT ( 'NONE',  ( -5.000000000000000888, 22.00000000000000000, 169.9999999999999716 ) ) ;
#3220 = CARTESIAN_POINT ( 'NONE',  ( 3.971273688083300613, 53.05572982463418441, 24.68326415769028159 ) ) ;
#3221 = CARTESIAN_POINT ( 'NONE',  ( 6.899297396606579369, 27.24035709017728379, 88.77211908039561195 ) ) ;
#3222 = CARTESIAN_POINT ( 'NONE',  ( 5.000000000000000888, 49.66980702654861801, -24.49489742783178059 ) ) ;
#3223 = CARTESIAN_POINT ( 'NONE',  ( 34.99999999999999289, 20.00000000000000355, 99.99999999999997158 ) ) ;
#3224 = CARTESIAN_POINT ( 'NONE',  ( -4.968239015973206385, 50.65284130285913022, 20.40394647430411723 ) ) ;
#3225 = CARTESIAN_POINT ( 'NONE',  ( -4.486710833798473352, 47.78725105462267209, 27.63829844907263222 ) ) ;
#3226 = VECTOR ( 'NONE', #2640, 1000.000000000000000 ) ;
#3227 = CARTESIAN_POINT ( 'NONE',  ( 42.47500000054622404, 13.80429023900056684, 86.29171490190961435 ) ) ;
#3228 = CARTESIAN_POINT ( 'NONE',  ( 1.137587760790131908, 45.12834422743500085, 20.96978904175466596 ) ) ;
#3229 = ORIENTED_EDGE ( 'NONE', *, *, #6546, .T. ) ;
#3230 = CARTESIAN_POINT ( 'NONE',  ( -8.964101468300798459, 15.55575854408322556, -26.52680384688584070 ) ) ;
#3231 = ADVANCED_FACE ( 'NONE', ( #5136 ), #6271, .T. ) ;
#3232 = CARTESIAN_POINT ( 'NONE',  ( 23.97500000054622049, 17.63344945572769973, 98.07665518445361386 ) ) ;
#3233 = CARTESIAN_POINT ( 'NONE',  ( 46.37500000054621552, 12.34168156654572535, 90.79316153445363113 ) ) ;
#3234 = CARTESIAN_POINT ( 'NONE',  ( 33.17500000054622689, 26.92701409722686634, 88.54243821818162985 ) ) ;
#3235 = AXIS2_PLACEMENT_3D ( 'NONE', #3070, #11824, #2372 ) ;
#3236 = DIRECTION ( 'NONE',  ( 0.000000000000000000, 0.000000000000000000, 1.000000000000000000 ) ) ;
#3237 = CARTESIAN_POINT ( 'NONE',  ( -2.000000000000015543, 20.00000000000000355, 90.79316153445363113 ) ) ;
#3238 = CARTESIAN_POINT ( 'NONE',  ( 28.07500000054622902, 13.80429023900056507, 95.29460816699764791 ) ) ;
#3239 = ORIENTED_EDGE ( 'NONE', *, *, #9768, .T. ) ;
#3240 = LINE ( 'NONE', #2289, #1237 ) ;
#3241 = ORIENTED_EDGE ( 'NONE', *, *, #697, .T. ) ;
#3242 = ORIENTED_EDGE ( 'NONE', *, *, #11448, .T. ) ;
#3243 = CARTESIAN_POINT ( 'NONE',  ( -21.00000000000001066, 77.00000000000000000, 166.8533255156881694 ) ) ;
#3244 = ORIENTED_EDGE ( 'NONE', *, *, #2314, .F. ) ;
#3245 = EDGE_CURVE ( 'NONE', #11306, #2044, #10375, .T. ) ;
#3246 = CARTESIAN_POINT ( 'NONE',  ( 38.67500000054622689, 15.71886984736413773, 84.90069139318163138 ) ) ;
#3247 = CARTESIAN_POINT ( 'NONE',  ( -8.665812433443574132E-16, 55.00000000000000000, -28.00000000000000355 ) ) ;
#3248 = EDGE_CURVE ( 'NONE', #8599, #850, #7151, .T. ) ;
#3249 = CARTESIAN_POINT ( 'NONE',  ( 19.65000000109246514, 20.00000000000000355, 98.29316153445363113 ) ) ;
#3250 = CARTESIAN_POINT ( 'NONE',  ( 38.07500000054622546, 15.71886984736413417, 96.68563167572563088 ) ) ;
#3251 = CARTESIAN_POINT ( 'NONE',  ( 37.29999999999998295, 26.37988106264029398, 86.15790661882942914 ) ) ;
#3252 = CARTESIAN_POINT ( 'NONE',  ( 49.07500000054622546, 26.19570976099943493, 86.29171490190961435 ) ) ;
#3253 = ORIENTED_EDGE ( 'NONE', *, *, #9260, .F. ) ;
#3254 = CARTESIAN_POINT ( 'NONE',  ( 22.35000000109246443, 13.62011893735971135, 86.15790661882942914 ) ) ;
#3255 = CARTESIAN_POINT ( 'NONE',  ( -4.744071016079746350, 48.38731143956220393, 24.54607980264442091 ) ) ;
#3256 = EDGE_LOOP ( 'NONE', ( #966, #4016, #6102, #4910 ) ) ;
#3257 =( BOUNDED_CURVE ( )  B_SPLINE_CURVE ( 2, ( #1823, #4937, #2974, #2780, #6840, #2909, #6642, #6708, #5709, #4751, #4816 ),
 .UNSPECIFIED., .F., .F. ) 
 B_SPLINE_CURVE_WITH_KNOTS ( ( 3, 2, 2, 2, 2, 3 ),
 ( 0.7666666666666666075, 0.7733333333333332060, 0.7799999999999999156, 0.7866666666666666252, 0.7933333333333333348, 0.8000000000000000444 ),
 .UNSPECIFIED. ) 
 CURVE ( )  GEOMETRIC_REPRESENTATION_ITEM ( )  RATIONAL_B_SPLINE_CURVE ( ( 1.000000000000000888, 0.9510565162951527540, 1.000000000000000000, 0.9510565162951535312, 1.000000000000000000, 0.9510565162951535312, 1.000000000000000000, 0.9510565162951535312, 1.000000000000000000, 0.9510565162951535312, 1.000000000000000000 ) ) 
 REPRESENTATION_ITEM ( '' )  );
#3258 = DIRECTION ( 'NONE',  ( -0.000000000000000000, -0.000000000000000000, -1.000000000000000000 ) ) ;
#3259 = ORIENTED_EDGE ( 'NONE', *, *, #12481, .F. ) ;
#3260 = VECTOR ( 'NONE', #2532, 1000.000000000000000 ) ;
#3261 = DIRECTION ( 'NONE',  ( -1.000000000000000000, 0.000000000000000000, -0.000000000000000000 ) ) ;
#3262 = B_SPLINE_CURVE_WITH_KNOTS ( 'NONE', 3,
 ( #494, #4295, #6386, #4359, #2515, #11083, #4481, #3468, #8233, #3402, #6202, #11142, #7332, #5193, #3340, #5317, #1322, #9251, #7272, #6262, #4236, #2449, #6324, #8295, #10194, #2388 ),
 .UNSPECIFIED., .F., .F.,
 ( 4, 2, 2, 2, 2, 2, 2, 2, 2, 2, 2, 2, 4 ),
 ( 0.01580376012220196039, 0.01679085241551835084, 0.01777794470883474129, 0.01975212929546752219, 0.02172631388210030656, 0.02271340617541669701, 0.02370049846873308746, 0.02567468305536586837, 0.02666177534868225882, 0.02764886764199864927, 0.02962305222863143364, 0.03061014452194782409, 0.03159723681526421801 ),
 .UNSPECIFIED. ) ;
#3263 = PLANE ( 'NONE',  #8460 ) ;
#3264 = B_SPLINE_CURVE_WITH_KNOTS ( 'NONE', 3,
 ( #11410, #1948, #6583, #2778, #2720, #4685, #4619, #877, #2907, #4748, #8556, #6771, #8615, #10636, #11470, #4875, #3855, #12484, #3790, #10447 ),
 .UNSPECIFIED., .F., .F.,
 ( 4, 2, 2, 2, 2, 2, 2, 2, 2, 4 ),
 ( 3.491326639452381067E-19, 0.0009808062029949312765, 0.001961612405989862119, 0.002942418608984793179, 0.003923224811979723371, 0.004904031014974653997, 0.005884837217969585491, 0.006375240319467059477, 0.006865643420964533464, 0.007846449623959500519 ),
 .UNSPECIFIED. ) ;
#3265 = FACE_OUTER_BOUND ( 'NONE', #6855, .T. ) ;
#3266 = EDGE_CURVE ( 'NONE', #5090, #10068, #1264, .T. ) ;
#3267 = CARTESIAN_POINT ( 'NONE',  ( 30.27500000054623186, 12.34168156654572535, 90.79316153445363113 ) ) ;
#3268 = CARTESIAN_POINT ( 'NONE',  ( 33.47500000054622404, 26.92701409722686634, 93.04388485072563242 ) ) ;
#3269 = FACE_OUTER_BOUND ( 'NONE', #12507, .T. ) ;
#3270 = CARTESIAN_POINT ( 'NONE',  ( 22.15000000109246514, 12.11403331821300533, 90.79316153445363113 ) ) ;
#3271 = ORIENTED_EDGE ( 'NONE', *, *, #11604, .F. ) ;
#3272 = AXIS2_PLACEMENT_3D ( 'NONE', #8318, #575, #12187 ) ;
#3273 = EDGE_CURVE ( 'NONE', #8883, #2615, #4476, .T. ) ;
#3274 = CARTESIAN_POINT ( 'NONE',  ( 42.55000000109245661, 17.56310227825321135, 83.29316153445363113 ) ) ;
#3275 = PLANE ( 'NONE',  #8884 ) ;
#3276 = VERTEX_POINT ( 'NONE', #1206 ) ;
#3277 = CARTESIAN_POINT ( 'NONE',  ( 45.00000000000000000, 20.00000000000000711, 197.9999999999999716 ) ) ;
#3278 = ORIENTED_EDGE ( 'NONE', *, *, #4367, .T. ) ;
#3279 = CARTESIAN_POINT ( 'NONE',  ( -6.608660176926854923, 12.46713484822145190, -24.11541629257941111 ) ) ;
#3280 = CARTESIAN_POINT ( 'NONE',  ( -8.651571107376318182, 25.02565239439968536, 23.45586713013333124 ) ) ;
#3281 = EDGE_CURVE ( 'NONE', #10732, #8970, #9129, .T. ) ;
#3282 = DIRECTION ( 'NONE',  ( -1.000000000000000000, -0.000000000000000000, -0.000000000000000000 ) ) ;
#3283 = FILL_AREA_STYLE_COLOUR ( '', #1958 ) ;
#3284 = CARTESIAN_POINT ( 'NONE',  ( 1.500000000000001332, 0.000000000000000000, 0.000000000000000000 ) ) ;
#3285 = PLANE ( 'NONE',  #9702 ) ;
#3286 = CARTESIAN_POINT ( 'NONE',  ( 2.562745747226488176E-15, 30.00000000000001066, 21.00000000000000000 ) ) ;
#3287 = CARTESIAN_POINT ( 'NONE',  ( 3.429011071898990822E-15, 55.00000000000000000, 28.00000000000000355 ) ) ;
#3288 = CARTESIAN_POINT ( 'NONE',  ( -4.839543938134134748, 48.70089194556705792, 27.57867091635483447 ) ) ;
#3289 = CARTESIAN_POINT ( 'NONE',  ( 0.6529056306158902423, 45.03187583116404369, 20.99234021528525318 ) ) ;
#3290 = EDGE_LOOP ( 'NONE', ( #7015, #11290, #10903, #1705 ) ) ;
#3291 = CARTESIAN_POINT ( 'NONE',  ( -9.917679487371039215, 18.67710825656768492, -26.18474513470922460 ) ) ;
#3292 = CARTESIAN_POINT ( 'NONE',  ( 28.89999999999998437, 17.56310227825320425, 83.29316153445363113 ) ) ;
#3293 = CARTESIAN_POINT ( 'NONE',  ( 43.47500000054622404, 26.92701409722686634, 93.04388485072563242 ) ) ;
#3294 = CARTESIAN_POINT ( 'NONE',  ( 26.47500000054622760, 13.80429023900056684, 86.29171490190961435 ) ) ;
#3295 = CARTESIAN_POINT ( 'NONE',  ( 9.410854331999907174, 16.58509554716785317, 97.48886294417630438 ) ) ;
#3296 = LINE ( 'NONE', #9140, #8370 ) ;
#3297 = DIRECTION ( 'NONE',  ( 0.000000000000000000, -0.5000000000000011102, -0.8660254037844379305 ) ) ;
#3298 = CARTESIAN_POINT ( 'NONE',  ( 26.87500000054622618, 22.36655054427230382, 83.50966788445364841 ) ) ;
#3299 = ORIENTED_EDGE ( 'NONE', *, *, #9336, .F. ) ;
#3300 = CARTESIAN_POINT ( 'NONE',  ( 23.05000000109246372, 27.13292387221364876, 88.47553407664153724 ) ) ;
#3301 = VERTEX_POINT ( 'NONE', #437 ) ;
#3302 = LINE ( 'NONE', #1281, #9961 ) ;
#3303 = ORIENTED_EDGE ( 'NONE', *, *, #5968, .F. ) ;
#3304 = CIRCLE ( 'NONE', #6938, 10.00000000000000355 ) ;
#3305 = CARTESIAN_POINT ( 'NONE',  ( 35.27500000054622120, 26.92701409722686634, 88.54243821818162985 ) ) ;
#3306 = DIRECTION ( 'NONE',  ( 0.000000000000000000, 0.000000000000000000, -1.000000000000000000 ) ) ;
#3307 = CARTESIAN_POINT ( 'NONE',  ( 20.45000000109246585, 15.59161060780646046, 84.72553407664153724 ) ) ;
#3308 = CARTESIAN_POINT ( 'NONE',  ( 31.27500000054622831, 26.92701409722686634, 88.54243821818162985 ) ) ;
#3309 = CARTESIAN_POINT ( 'NONE',  ( 34.19999999999998863, 15.59161060780645691, 96.86078899226572503 ) ) ;
#3310 = EDGE_CURVE ( 'NONE', #2251, #11822, #12002, .T. ) ;
#3311 = CARTESIAN_POINT ( 'NONE',  ( 42.97500000054623115, 24.28113015263587471, 84.90069139318163138 ) ) ;
#3312 = VERTEX_POINT ( 'NONE', #10142 ) ;
#3313 = VECTOR ( 'NONE', #946, 1000.000000000000000 ) ;
#3314 = CARTESIAN_POINT ( 'NONE',  ( 22.05000000109246372, 12.86707612778636012, 93.11078899226572503 ) ) ;
#3315 = CARTESIAN_POINT ( 'NONE',  ( -9.918789871757258680, 18.68607266337350836, 22.94817778295035993 ) ) ;
#3316 = ORIENTED_EDGE ( 'NONE', *, *, #1038, .T. ) ;
#3317 = CARTESIAN_POINT ( 'NONE',  ( -9.356538917183957693, 23.54422275815007382, -26.39077148263137218 ) ) ;
#3318 = CARTESIAN_POINT ( 'NONE',  ( 36.85000000109246798, 24.40838939219355197, 84.72553407664153724 ) ) ;
#3319 = ORIENTED_EDGE ( 'NONE', *, *, #7383, .T. ) ;
#3320 = CARTESIAN_POINT ( 'NONE',  ( -2.000000000000015543, 20.00000000000000355, 90.79316153445363113 ) ) ;
#3321 = CARTESIAN_POINT ( 'NONE',  ( 36.45000000109246940, 15.59161060780646046, 84.72553407664153724 ) ) ;
#3322 = DIRECTION ( 'NONE',  ( -1.000000000000000000, 0.000000000000000000, 0.000000000000000000 ) ) ;
#3323 = AXIS2_PLACEMENT_3D ( 'NONE', #9168, #9358, #3385 ) ;
#3324 = CARTESIAN_POINT ( 'NONE',  ( 28.07500000054622902, 13.80429023900056507, 95.29460816699764791 ) ) ;
#3325 = CARTESIAN_POINT ( 'NONE',  ( 22.17500000054622333, 13.80429023900056507, 95.29460816699764791 ) ) ;
#3326 = AXIS2_PLACEMENT_3D ( 'NONE', #1612, #5492, #2624 ) ;
#3327 = DIRECTION ( 'NONE',  ( -1.000000000000000000, -0.000000000000000000, -0.000000000000000000 ) ) ;
#3328 =( BOUNDED_CURVE ( )  B_SPLINE_CURVE ( 3, ( #12303, #11039, #3360, #7229 ),
 .UNSPECIFIED., .F., .F. ) 
 B_SPLINE_CURVE_WITH_KNOTS ( ( 4, 4 ),
 ( 3.141592653589793116, 4.712388980384689674 ),
 .UNSPECIFIED. ) 
 CURVE ( )  GEOMETRIC_REPRESENTATION_ITEM ( )  RATIONAL_B_SPLINE_CURVE ( ( 1.000000000000000000, 0.8047378541243649375, 0.8047378541243649375, 1.000000000000000000 ) ) 
 REPRESENTATION_ITEM ( '' )  );
#3329 = PLANE ( 'NONE',  #571 ) ;
#3330 = ORIENTED_EDGE ( 'NONE', *, *, #3811, .F. ) ;
#3331 = CARTESIAN_POINT ( 'NONE',  ( 44.55000000109245661, 17.56310227825321135, 83.29316153445363113 ) ) ;
#3332 = CARTESIAN_POINT ( 'NONE',  ( 4.967652032308136789, 50.65502714036492904, -24.50156428836015721 ) ) ;
#3333 = ORIENTED_EDGE ( 'NONE', *, *, #7811, .F. ) ;
#3334 = CARTESIAN_POINT ( 'NONE',  ( 47.49999999999997868, 27.88596668178699645, 90.79316153445363113 ) ) ;
#3335 = EDGE_CURVE ( 'NONE', #2279, #3004, #10902, .T. ) ;
#3336 = ORIENTED_EDGE ( 'NONE', *, *, #6601, .F. ) ;
#3337 = CARTESIAN_POINT ( 'NONE',  ( -8.659888037695356644, 14.95771684574014948, -19.13532407230401944 ) ) ;
#3338 = CARTESIAN_POINT ( 'NONE',  ( -2.619138840591237472, 29.67330545628644600, 24.87083797681799169 ) ) ;
#3339 = CARTESIAN_POINT ( 'NONE',  ( 0.000000000000000000, 4.685197434473814759, -5.637851296924623057E-15 ) ) ;
#3340 = CARTESIAN_POINT ( 'NONE',  ( -7.945999201647152788, 13.89399703635140249, 23.70671076423498391 ) ) ;
#3341 = CARTESIAN_POINT ( 'NONE',  ( 5.000000000000000000, -4.685197434473812983, 6.938893903907228378E-15 ) ) ;
#3342 = CIRCLE ( 'NONE', #11654, 8.400000000000000355 ) ;
#3343 = CARTESIAN_POINT ( 'NONE',  ( -6.197539731915355238E-14, 9.999999999999182876, 21.00000000000039080 ) ) ;
#3344 = CARTESIAN_POINT ( 'NONE',  ( -10.00000000000000355, 20.00000000000000355, 109.9999999999999858 ) ) ;
#3345 = DIRECTION ( 'NONE',  ( 0.000000000000000000, 0.000000000000000000, -1.000000000000000000 ) ) ;
#3346 = ADVANCED_FACE ( 'NONE', ( #6452, #4548 ), #7403, .F. ) ;
#3347 = CARTESIAN_POINT ( 'NONE',  ( -1.301064515050044168, 45.16113941612564275, -24.96819193944210724 ) ) ;
#3348 = ORIENTED_EDGE ( 'NONE', *, *, #490, .F. ) ;
#3349 = CARTESIAN_POINT ( 'NONE',  ( -6.611445631918658528, 12.46901802506235413, -27.21243546183779216 ) ) ;
#3350 = CONTEXT_DEPENDENT_SHAPE_REPRESENTATION ( #6270, #6199 ) ;
#3351 = DIRECTION ( 'NONE',  ( 0.000000000000000000, 0.000000000000000000, 1.000000000000000000 ) ) ;
#3352 = ADVANCED_FACE ( 'NONE', ( #1747 ), #11341, .T. ) ;
#3353 = LINE ( 'NONE', #1459, #7836 ) ;
#3354 = CARTESIAN_POINT ( 'NONE',  ( 42.57500000054622546, 13.80429023900056684, 86.29171490190961435 ) ) ;
#3355 = CARTESIAN_POINT ( 'NONE',  ( 29.27500000054622831, 27.65831843345427998, 90.79316153445363113 ) ) ;
#3356 = CARTESIAN_POINT ( 'NONE',  ( 9.621280771571464996, 17.26369774818443759, 83.80577239012578161 ) ) ;
#3357 = FACE_OUTER_BOUND ( 'NONE', #1466, .T. ) ;
#3358 = AXIS2_PLACEMENT_3D ( 'NONE', #11854, #5953, #9128 ) ;
#3359 = CARTESIAN_POINT ( 'NONE',  ( 35.09999999999998721, 22.43689772174679575, 83.29316153445363113 ) ) ;
#3360 = CARTESIAN_POINT ( 'NONE',  ( -32.89339828220179385, 69.50000000000000000, 151.2467237978899846 ) ) ;
#3361 = EDGE_CURVE ( 'NONE', #9944, #11196, #11592, .T. ) ;
#3362 = EDGE_LOOP ( 'NONE', ( #282, #9226, #9843, #2371 ) ) ;
#3363 = CARTESIAN_POINT ( 'NONE',  ( -111.8465843842649292, 77.00000000000000000, 101.8533255156881978 ) ) ;
#3364 = ORIENTED_EDGE ( 'NONE', *, *, #5202, .F. ) ;
#3365 = DIRECTION ( 'NONE',  ( -1.000000000000000000, -0.000000000000000000, -0.000000000000000000 ) ) ;
#3366 = ORIENTED_EDGE ( 'NONE', *, *, #2341, .F. ) ;
#3367 = CARTESIAN_POINT ( 'NONE',  ( 34.07500000054622546, 15.71886984736413417, 96.68563167572563088 ) ) ;
#3368 = CARTESIAN_POINT ( 'NONE',  ( -6.197539731915355238E-14, 9.999999999999182876, 21.00000000000039080 ) ) ;
#3369 = CARTESIAN_POINT ( 'NONE',  ( 45.97500000054623115, 15.71886984736413417, 96.68563167572563088 ) ) ;
#3370 = SHAPE_REPRESENTATION ( 'socket head cap screw_iso_ISO 4762 M12 x 20 - 20N', ( #9021 ), #708 ) ;
#3371 = CARTESIAN_POINT ( 'NONE',  ( 36.47500000054622404, 13.07298590277314432, 88.54243821818161564 ) ) ;
#3372 = CARTESIAN_POINT ( 'NONE',  ( 34.79999999999999005, 15.59161060780646046, 84.72553407664153724 ) ) ;
#3373 = CARTESIAN_POINT ( 'NONE',  ( 46.67500000054623399, 17.63344945572770328, 83.50966788445364841 ) ) ;
#3374 = VERTEX_POINT ( 'NONE', #2708 ) ;
#3375 = CARTESIAN_POINT ( 'NONE',  ( 23.35000000109246798, 26.37988106264029398, 95.42841645007781892 ) ) ;
#3376 = CARTESIAN_POINT ( 'NONE',  ( 92.00000000000000000, 0.000000000000000000, 5.035999999999999588 ) ) ;
#3377 = AXIS2_PLACEMENT_3D ( 'NONE', #12111, #7282, #3534 ) ;
#3378 = ORIENTED_EDGE ( 'NONE', *, *, #5111, .F. ) ;
#3379 = DIRECTION ( 'NONE',  ( 1.000000000000000000, 0.000000000000000000, 0.000000000000000000 ) ) ;
#3380 = VERTEX_POINT ( 'NONE', #8422 ) ;
#3381 = FACE_OUTER_BOUND ( 'NONE', #5742, .T. ) ;
#3382 = CARTESIAN_POINT ( 'NONE',  ( 36.99999999999999289, 20.00000000000000355, 83.29316153445364534 ) ) ;
#3383 = CARTESIAN_POINT ( 'NONE',  ( 6.000000000000000000, -4.379923479639802331, -2.528749999999991616 ) ) ;
#3384 = EDGE_CURVE ( 'NONE', #7013, #9272, #4628, .T. ) ;
#3385 = DIRECTION ( 'NONE',  ( 0.000000000000000000, 0.000000000000000000, 1.000000000000000000 ) ) ;
#3386 = VECTOR ( 'NONE', #2652, 999.9999999999998863 ) ;
#3387 = CARTESIAN_POINT ( 'NONE',  ( 22.37500000054622973, 13.07298590277314432, 88.54243821818161564 ) ) ;
#3388 = CARTESIAN_POINT ( 'NONE',  ( 24.17500000054622689, 13.80429023900056507, 95.29460816699764791 ) ) ;
#3389 = CARTESIAN_POINT ( 'NONE',  ( 10.00000000000000000, 20.66692791361947812, 26.15339366124403853 ) ) ;
#3390 = CARTESIAN_POINT ( 'NONE',  ( 21.95000000109245875, 13.62011893735970958, 95.42841645007781892 ) ) ;
#3391 = EDGE_LOOP ( 'NONE', ( #530, #5759, #12470, #11713, #8982 ) ) ;
#3392 = CARTESIAN_POINT ( 'NONE',  ( 45.05000000109246372, 27.13292387221364876, 88.47553407664153724 ) ) ;
#3393 = LINE ( 'NONE', #2380, #3413 ) ;
#3394 = ORIENTED_EDGE ( 'NONE', *, *, #11734, .T. ) ;
#3395 = DIRECTION ( 'NONE',  ( 0.000000000000000000, 0.000000000000000000, -1.000000000000000000 ) ) ;
#3396 = VERTEX_POINT ( 'NONE', #9503 ) ;
#3397 = VECTOR ( 'NONE', #6686, 1000.000000000000000 ) ;
#3398 = CARTESIAN_POINT ( 'NONE',  ( 5.000000000000000000, 50.00000000000000000, 20.39607805437114152 ) ) ;
#3399 = CARTESIAN_POINT ( 'NONE',  ( -6.109221465413982699, 27.94329460785578689, 24.24832107967536388 ) ) ;
#3400 = CARTESIAN_POINT ( 'NONE',  ( 3.045782272221063902, 53.96862488584907425, 24.81409817615884705 ) ) ;
#3401 = EDGE_CURVE ( 'NONE', #11790, #4895, #2028, .T. ) ;
#3402 = CARTESIAN_POINT ( 'NONE',  ( -5.845694806184612347, 11.88009017893230990, 24.30851799965319060 ) ) ;
#3403 = CARTESIAN_POINT ( 'NONE',  ( 6.000000000000000000, -5.839897972853063557, 6.938893903907228378E-15 ) ) ;
#3404 = CARTESIAN_POINT ( 'NONE',  ( -4.478749722781300235, 11.03480093803115558, 20.52614747825679942 ) ) ;
#3405 = CARTESIAN_POINT ( 'NONE',  ( 5.000000000000000000, -2.342598717236911821, -4.057499999999996554 ) ) ;
#3406 = DIRECTION ( 'NONE',  ( 1.000000000000000000, 0.000000000000000000, 0.000000000000000000 ) ) ;
#3407 = PRODUCT_RELATED_PRODUCT_CATEGORY ( 'part', '', ( #10963 ) ) ;
#3408 = ADVANCED_FACE ( 'NONE', ( #2521 ), #681, .T. ) ;
#3409 = CARTESIAN_POINT ( 'NONE',  ( 47.35000000109245377, 26.37988106264029398, 95.42841645007781892 ) ) ;
#3410 = VERTEX_POINT ( 'NONE', #6511 ) ;
#3411 = AXIS2_PLACEMENT_3D ( 'NONE', #1122, #4987, #3076 ) ;
#3412 = ITEM_DEFINED_TRANSFORMATION ( 'NONE', 'NONE', #5761,  #9021 ) ;
#3413 = VECTOR ( 'NONE', #422, 1000.000000000000000 ) ;
#3414 = CYLINDRICAL_SURFACE ( 'NONE', #9057, 7.499999999999992895 ) ;
#3415 = CARTESIAN_POINT ( 'NONE',  ( 0.6550203249928933102, 54.96765362015771927, 24.99347278016167095 ) ) ;
#3416 = CARTESIAN_POINT ( 'NONE',  ( 44.37500000054622262, 12.34168156654572535, 90.79316153445363113 ) ) ;
#3417 = EDGE_CURVE ( 'NONE', #2160, #12416, #5449, .T. ) ;
#3418 = CARTESIAN_POINT ( 'NONE',  ( 29.37500000054622973, 26.92701409722686634, 93.04388485072563242 ) ) ;
#3419 = VECTOR ( 'NONE', #4237, 1000.000000000000000 ) ;
#3420 = CARTESIAN_POINT ( 'NONE',  ( 10.00000000000000533, 19.67046583110989744, -22.91287847477920181 ) ) ;
#3421 = CARTESIAN_POINT ( 'NONE',  ( -31.74999999999995737, 6.123233995736767268E-16, -5.000000000000000888 ) ) ;
#3422 = CARTESIAN_POINT ( 'NONE',  ( 6.000000000000000000, 0.000000000000000000, 0.000000000000000000 ) ) ;
#3423 = CARTESIAN_POINT ( 'NONE',  ( -111.8465843842649292, 77.00000000000000000, 146.8533255156881978 ) ) ;
#3424 = ORIENTED_EDGE ( 'NONE', *, *, #12017, .T. ) ;
#3425 = ADVANCED_FACE ( 'NONE', ( #2833 ), #3648, .F. ) ;
#3426 = DIRECTION ( 'NONE',  ( 0.000000000000000000, 0.000000000000000000, 1.000000000000000000 ) ) ;
#3427 = ORIENTED_EDGE ( 'NONE', *, *, #8133, .T. ) ;
#3428 = DIRECTION ( 'NONE',  ( -0.000000000000000000, -0.000000000000000000, 1.000000000000000000 ) ) ;
#3429 = ORIENTED_EDGE ( 'NONE', *, *, #2334, .T. ) ;
#3430 =( NAMED_UNIT ( * ) PLANE_ANGLE_UNIT ( ) SI_UNIT ( $, .RADIAN. ) );
#3431 = AXIS2_PLACEMENT_3D ( 'NONE', #11099, #8372, #6282 ) ;
#3432 = ADVANCED_FACE ( 'NONE', ( #5105 ), #283, .F. ) ;
#3433 = EDGE_CURVE ( 'NONE', #10935, #2736, #5699, .T. ) ;
#3434 = AXIS2_PLACEMENT_3D ( 'NONE', #5669, #12449, #9538 ) ;
#3435 = CARTESIAN_POINT ( 'NONE',  ( 32.97500000054621694, 22.36655054427230382, 83.50966788445364841 ) ) ;
#3436 = PLANE ( 'NONE',  #4716 ) ;
#3437 = CARTESIAN_POINT ( 'NONE',  ( 43.67500000054621978, 22.36655054427230027, 98.07665518445361386 ) ) ;
#3438 = CARTESIAN_POINT ( 'NONE',  ( 32.27500000054622831, 13.07298590277314254, 93.04388485072563242 ) ) ;
#3439 = CARTESIAN_POINT ( 'NONE',  ( 37.09999999999998010, 22.43689772174679575, 83.29316153445363113 ) ) ;
#3440 = CARTESIAN_POINT ( 'NONE',  ( -7.515231585295850891, 26.60501645963920225, 19.61046409729162932 ) ) ;
#3441 = CARTESIAN_POINT ( 'NONE',  ( 47.47500000054623115, 26.19570976099943493, 95.29460816699764791 ) ) ;
#3442 = VERTEX_POINT ( 'NONE', #9628 ) ;
#3443 = CARTESIAN_POINT ( 'NONE',  ( 28.05000000109246372, 12.86707612778636012, 93.11078899226572503 ) ) ;
#3444 = CARTESIAN_POINT ( 'NONE',  ( 12.59999999999999964, 0.000000000000000000, 0.000000000000000000 ) ) ;
#3445 = VERTEX_POINT ( 'NONE', #7785 ) ;
#3446 = CARTESIAN_POINT ( 'NONE',  ( -8.658590212363067806, 25.01362066216688262, 26.62809547983346548 ) ) ;
#3447 = ORIENTED_EDGE ( 'NONE', *, *, #4084, .F. ) ;
#3448 = DIRECTION ( 'NONE',  ( 0.000000000000000000, 0.000000000000000000, 1.000000000000000000 ) ) ;
#3449 = FACE_OUTER_BOUND ( 'NONE', #6539, .T. ) ;
#3450 = DIRECTION ( 'NONE',  ( 1.000000000000000000, 0.000000000000000000, 0.000000000000000000 ) ) ;
#3451 =( BOUNDED_CURVE ( )  B_SPLINE_CURVE ( 2, ( #6735, #5034, #8832, #11631, #3884, #9731, #6992, #4908, #10600, #1913, #87 ),
 .UNSPECIFIED., .F., .F. ) 
 B_SPLINE_CURVE_WITH_KNOTS ( ( 3, 2, 2, 2, 2, 3 ),
 ( 0.1333333333333334425, 0.1400000000000000966, 0.1466666666666666952, 0.1533333333333333215, 0.1599999999999999756, 0.1666666666666665741 ),
 .UNSPECIFIED. ) 
 CURVE ( )  GEOMETRIC_REPRESENTATION_ITEM ( )  RATIONAL_B_SPLINE_CURVE ( ( 0.9999999999999992228, 0.9510565162951543083, 1.000000000000000000, 0.9510565162951535312, 1.000000000000000000, 0.9510565162951535312, 1.000000000000000000, 0.9510565162951535312, 1.000000000000000000, 0.9510565162951541973, 0.9999999999999993339 ) ) 
 REPRESENTATION_ITEM ( '' )  );
#3452 = CIRCLE ( 'NONE', #5685, 4.057500000000000107 ) ;
#3453 = FACE_OUTER_BOUND ( 'NONE', #2472, .T. ) ;
#3454 = CARTESIAN_POINT ( 'NONE',  ( 21.97500000054622760, 15.71886984736413417, 96.68563167572563088 ) ) ;
#3455 = CARTESIAN_POINT ( 'NONE',  ( 24.77500000054622475, 17.63344945572770328, 83.50966788445364841 ) ) ;
#3456 = LINE ( 'NONE', #9110, #6373 ) ;
#3457 = DIRECTION ( 'NONE',  ( -0.000000000000000000, 0.000000000000000000, -1.000000000000000000 ) ) ;
#3458 = ORIENTED_EDGE ( 'NONE', *, *, #7225, .F. ) ;
#3459 = CARTESIAN_POINT ( 'NONE',  ( 41.65000000109246514, 20.00000000000000355, 98.29316153445363113 ) ) ;
#3460 = VERTEX_POINT ( 'NONE', #4737 ) ;
#3461 = CARTESIAN_POINT ( 'NONE',  ( 0.000000000000000000, -3.000000000000003109, 25.00000000000000355 ) ) ;
#3462 = AXIS2_PLACEMENT_3D ( 'NONE', #4377, #3426, #4191 ) ;
#3463 = VERTEX_POINT ( 'NONE', #11893 ) ;
#3464 = CARTESIAN_POINT ( 'NONE',  ( -10.00000000000000355, 19.66998333124466214, -22.91287847477919826 ) ) ;
#3465 = CARTESIAN_POINT ( 'NONE',  ( -1.002883791299520887E-19, 10.00000000000000000, -25.00000000000000000 ) ) ;
#3466 = CARTESIAN_POINT ( 'NONE',  ( 29.19999999999998508, 24.40838939219355197, 84.72553407664153724 ) ) ;
#3467 =( NAMED_UNIT ( * ) PLANE_ANGLE_UNIT ( ) SI_UNIT ( $, .RADIAN. ) );
#3468 = CARTESIAN_POINT ( 'NONE',  ( -4.466051270639568749, 11.02833005318139925, 24.60558887372674519 ) ) ;
#3469 = FACE_BOUND ( 'NONE', #3683, .T. ) ;
#3470 = CARTESIAN_POINT ( 'NONE',  ( 6.000000000000000000, 4.379923479639795225, -2.528750000000006271 ) ) ;
#3471 = CYLINDRICAL_SURFACE ( 'NONE', #12424, 5.000000000000000000 ) ;
#3472 = ADVANCED_FACE ( 'NONE', ( #7596 ), #3778, .F. ) ;
#3473 = CARTESIAN_POINT ( 'NONE',  ( 5.303296350723960551, 28.48414319546200346, 24.43259468344301055 ) ) ;
#3474 = CARTESIAN_POINT ( 'NONE',  ( 23.59999999999999076, 27.13292387221364876, 93.11078899226573924 ) ) ;
#3475 = EDGE_LOOP ( 'NONE', ( #3637, #4801, #3531, #2066 ) ) ;
#3476 = CARTESIAN_POINT ( 'NONE',  ( 2.505975641493357831, 45.66085398937747186, 24.87560495202607669 ) ) ;
#3477 = CARTESIAN_POINT ( 'NONE',  ( 3.971273688083300613, 53.05572982463418441, 24.68326415769028159 ) ) ;
#3478 = CARTESIAN_POINT ( 'NONE',  ( 36.47500000054622404, 13.07298590277314432, 88.54243821818161564 ) ) ;
#3479 = CARTESIAN_POINT ( 'NONE',  ( 25.97500000054622760, 15.71886984736413417, 96.68563167572563088 ) ) ;
#3480 = CARTESIAN_POINT ( 'NONE',  ( 7.416892943932571924, 13.28747952548623878, 87.41303169954825592 ) ) ;
#3481 = CARTESIAN_POINT ( 'NONE',  ( 6.999999999999978684, 20.00000000000000355, 109.9999999999999858 ) ) ;
#3482 = CARTESIAN_POINT ( 'NONE',  ( 35.59999999999998721, 27.13292387221364876, 93.11078899226573924 ) ) ;
#3483 = ORIENTED_EDGE ( 'NONE', *, *, #6675, .F. ) ;
#3484 = LINE ( 'NONE', #7354, #7915 ) ;
#3485 = ORIENTED_EDGE ( 'NONE', *, *, #833, .F. ) ;
#3486 = CARTESIAN_POINT ( 'NONE',  ( 0.000000000000000000, 20.00000000000000355, 109.9999999999999858 ) ) ;
#3487 = ADVANCED_FACE ( 'NONE', ( #10501 ), #8547, .T. ) ;
#3488 = DIRECTION ( 'NONE',  ( 0.000000000000000000, 0.000000000000000000, 1.000000000000000000 ) ) ;
#3489 = CARTESIAN_POINT ( 'NONE',  ( 30.57500000054622191, 13.80429023900056684, 86.29171490190961435 ) ) ;
#3490 = CARTESIAN_POINT ( 'NONE',  ( -5.000000000000000000, 50.33010793893004831, -27.54995462791181993 ) ) ;
#3491 = CARTESIAN_POINT ( 'NONE',  ( 45.27500000054622831, 27.65831843345427998, 90.79316153445363113 ) ) ;
#3492 = CARTESIAN_POINT ( 'NONE',  ( 35.77500000054622831, 22.36655054427230027, 98.07665518445361386 ) ) ;
#3493 = CARTESIAN_POINT ( 'NONE',  ( 33.09999999999998010, 22.43689772174679575, 83.29316153445363113 ) ) ;
#3494 = CARTESIAN_POINT ( 'NONE',  ( -6.612279285637575832, 27.52949341102648262, 19.93770914801777749 ) ) ;
#3495 = CARTESIAN_POINT ( 'NONE',  ( 38.87500000054623683, 22.36655054427230382, 83.50966788445364841 ) ) ;
#3496 = ORIENTED_EDGE ( 'NONE', *, *, #9909, .T. ) ;
#3497 = CARTESIAN_POINT ( 'NONE',  ( 46.37500000054622973, 13.07298590277314432, 88.54243821818161564 ) ) ;
#3498 = CARTESIAN_POINT ( 'NONE',  ( 92.00000000000000000, 6.167321280506070407E-16, -5.035999999999999588 ) ) ;
#3499 = ORIENTED_EDGE ( 'NONE', *, *, #12097, .F. ) ;
#3500 = CARTESIAN_POINT ( 'NONE',  ( -9.108306422252258727, 24.14061933117464775, 26.47746754580360218 ) ) ;
#3501 = ORIENTED_EDGE ( 'NONE', *, *, #10069, .F. ) ;
#3502 = CIRCLE ( 'NONE', #6340, 5.057500000000000107 ) ;
#3503 = CYLINDRICAL_SURFACE ( 'NONE', #6572, 9.000000000000000000 ) ;
#3504 = DIRECTION ( 'NONE',  ( 0.000000000000000000, 0.8660254037844380415, -0.5000000000000012212 ) ) ;
#3505 = CARTESIAN_POINT ( 'NONE',  ( 10.00000000000000355, 20.00000000000000355, -28.00000000000000711 ) ) ;
#3506 = CARTESIAN_POINT ( 'NONE',  ( 31.65000000109246514, 20.00000000000000355, 98.29316153445363113 ) ) ;
#3507 = EDGE_CURVE ( 'NONE', #6002, #1521, #1235, .T. ) ;
#3508 = CARTESIAN_POINT ( 'NONE',  ( 21.07500000054622546, 26.19570976099943493, 86.29171490190961435 ) ) ;
#3509 = CARTESIAN_POINT ( 'NONE',  ( 23.77500000054622475, 22.36655054427230027, 98.07665518445361386 ) ) ;
#3510 = AXIS2_PLACEMENT_3D ( 'NONE', #7667, #5583, #2721 ) ;
#3511 = CARTESIAN_POINT ( 'NONE',  ( -50.00000000000001421, 77.00000000000000000, 101.8533255156881978 ) ) ;
#3512 = CARTESIAN_POINT ( 'NONE',  ( 0.000000000000000000, 139.9999999999999716, -25.00000000000000000 ) ) ;
#3513 = ORIENTED_EDGE ( 'NONE', *, *, #1524, .T. ) ;
#3514 = CARTESIAN_POINT ( 'NONE',  ( 44.35000000109246798, 13.62011893735971135, 86.15790661882942914 ) ) ;
#3515 = DIRECTION ( 'NONE',  ( -1.000000000000000000, -0.000000000000000000, -0.000000000000000000 ) ) ;
#3516 = ORIENTED_EDGE ( 'NONE', *, *, #6821, .T. ) ;
#3517 = CARTESIAN_POINT ( 'NONE',  ( 47.09999999999998010, 22.43689772174677088, 83.29316153445361692 ) ) ;
#3518 = ORIENTED_EDGE ( 'NONE', *, *, #6802, .T. ) ;
#3519 = DIRECTION ( 'NONE',  ( 0.000000000000000000, -1.000000000000000000, 0.000000000000000000 ) ) ;
#3520 = CARTESIAN_POINT ( 'NONE',  ( 1.648701702613829090, 10.13131270077370338, -24.94769321807935825 ) ) ;
#3521 = AXIS2_PLACEMENT_3D ( 'NONE', #11352, #5396, #11098 ) ;
#3522 = ORIENTED_EDGE ( 'NONE', *, *, #2113, .F. ) ;
#3523 = FACE_OUTER_BOUND ( 'NONE', #1815, .T. ) ;
#3524 = CARTESIAN_POINT ( 'NONE',  ( 38.45000000109246230, 15.59161060780646046, 84.72553407664153724 ) ) ;
#3525 = CARTESIAN_POINT ( 'NONE',  ( 22.19999999999998863, 15.59161060780645691, 96.86078899226572503 ) ) ;
#3526 = CARTESIAN_POINT ( 'NONE',  ( -5.049704742916529376, 11.34434628041953452, 20.39145111578409697 ) ) ;
#3527 = CARTESIAN_POINT ( 'NONE',  ( -9.983890631919367209, 19.34374299500451855, 26.15957060131868417 ) ) ;
#3528 = CARTESIAN_POINT ( 'NONE',  ( 29.57500000054622546, 24.28113015263587116, 96.68563167572563088 ) ) ;
#3529 = DIRECTION ( 'NONE',  ( 0.000000000000000000, 0.000000000000000000, -1.000000000000000000 ) ) ;
#3530 = DIRECTION ( 'NONE',  ( -0.000000000000000000, 0.8660254037844393737, 0.4999999999999987788 ) ) ;
#3531 = ORIENTED_EDGE ( 'NONE', *, *, #10882, .T. ) ;
#3532 = B_SPLINE_CURVE_WITH_KNOTS ( 'NONE', 3,
 ( #6811, #2883, #11701, #922, #4916, #12525, #3832, #3006, #5869, #1863, #7708, #6619, #10738, #2820, #11449, #2758, #10490, #2050, #5743, #1800, #6874, #10675, #5930, #8776 ),
 .UNSPECIFIED., .F., .F.,
 ( 4, 2, 2, 2, 2, 2, 2, 2, 2, 2, 2, 4 ),
 ( 5.438949063372056100E-19, 0.001975691086292785757, 0.002963536629439178418, 0.003951382172585572380, 0.005927073258878355969, 0.006914918802024747763, 0.007902764345171137822, 0.009878455431463928349, 0.01185414651775671888, 0.01284199206090311240, 0.01382983760404950767, 0.01580552869034228605 ),
 .UNSPECIFIED. ) ;
#3533 = ADVANCED_FACE ( 'NONE', ( #5700 ), #7658, .F. ) ;
#3534 = DIRECTION ( 'NONE',  ( 0.000000000000000000, 0.000000000000000000, -1.000000000000000000 ) ) ;
#3535 = EDGE_CURVE ( 'NONE', #5337, #2279, #7517, .T. ) ;
#3536 =( GEOMETRIC_REPRESENTATION_CONTEXT ( 3 ) GLOBAL_UNCERTAINTY_ASSIGNED_CONTEXT ( ( #951 ) ) GLOBAL_UNIT_ASSIGNED_CONTEXT ( ( #4583, #1604, #3625 ) ) REPRESENTATION_CONTEXT ( 'NONE', 'WORKASPACE' ) );
#3537 = CARTESIAN_POINT ( 'NONE',  ( 38.77500000054622831, 20.00000000000000355, 83.50966788445364841 ) ) ;
#3538 = CARTESIAN_POINT ( 'NONE',  ( 39.87500000054622262, 20.00000000000000355, 98.07665518445361386 ) ) ;
#3539 = CARTESIAN_POINT ( 'NONE',  ( 27.37500000054622973, 26.92701409722686634, 93.04388485072563242 ) ) ;
#3540 = AXIS2_PLACEMENT_3D ( 'NONE', #6558, #10887, #3213 ) ;
#3541 = CARTESIAN_POINT ( 'NONE',  ( 8.868804215452586348, 15.35919039895786220, 84.88169823822040883 ) ) ;
#3542 = CARTESIAN_POINT ( 'NONE',  ( 4.743169864344128683, 48.38453593858750423, 24.54625634892152775 ) ) ;
#3543 = CARTESIAN_POINT ( 'NONE',  ( -5.000000000000000000, 50.00000000000000000, -20.39607805437114152 ) ) ;
#3544 = CARTESIAN_POINT ( 'NONE',  ( 31.69999999999999218, 26.37988106264029398, 95.42841645007781892 ) ) ;
#3545 = ORIENTED_EDGE ( 'NONE', *, *, #8301, .F. ) ;
#3546 = CARTESIAN_POINT ( 'NONE',  ( 10.00000000000000533, 19.33140358361892552, 22.91287847477920891 ) ) ;
#3547 = ORIENTED_EDGE ( 'NONE', *, *, #4033, .F. ) ;
#3548 = DIRECTION ( 'NONE',  ( -0.000000000000000000, -1.000000000000000000, -0.000000000000000000 ) ) ;
#3549 = AXIS2_PLACEMENT_3D ( 'NONE', #6623, #4604, #1682 ) ;
#3550 = DIRECTION ( 'NONE',  ( 1.000000000000000000, 0.000000000000000000, 0.000000000000000000 ) ) ;
#3551 = CARTESIAN_POINT ( 'NONE',  ( 32.37500000054621552, 12.34168156654572357, 90.79316153445363113 ) ) ;
#3552 = LINE ( 'NONE', #7488, #2690 ) ;
#3553 = CARTESIAN_POINT ( 'NONE',  ( 43.47500000054623115, 26.19570976099943849, 95.29460816699764791 ) ) ;
#3554 = CARTESIAN_POINT ( 'NONE',  ( 35.07500000054622546, 24.28113015263587471, 84.90069139318163138 ) ) ;
#3555 = CARTESIAN_POINT ( 'NONE',  ( 27.99999999999998579, 20.00000000000000355, 98.29316153445363113 ) ) ;
#3556 = ADVANCED_FACE ( 'NONE', ( #3131 ), #5758, .F. ) ;
#3557 = CIRCLE ( 'NONE', #2137, 1.499999999999999556 ) ;
#3558 = CARTESIAN_POINT ( 'NONE',  ( 39.47500000054623115, 26.19570976099943493, 95.29460816699764791 ) ) ;
#3559 = VERTEX_POINT ( 'NONE', #6999 ) ;
#3560 = CARTESIAN_POINT ( 'NONE',  ( 21.45000000109246230, 24.40838939219354842, 96.86078899226572503 ) ) ;
#3561 = ORIENTED_EDGE ( 'NONE', *, *, #10397, .T. ) ;
#3562 = CARTESIAN_POINT ( 'NONE',  ( 2.295021694196371698, 10.26129700091049557, 20.87675788803829846 ) ) ;
#3563 = EDGE_CURVE ( 'NONE', #730, #7703, #11363, .T. ) ;
#3564 = ORIENTED_EDGE ( 'NONE', *, *, #10628, .F. ) ;
#3565 = LINE ( 'NONE', #6666, #2727 ) ;
#3566 = FACE_OUTER_BOUND ( 'NONE', #7971, .T. ) ;
#3567 = DIRECTION ( 'NONE',  ( 0.000000000000000000, 0.000000000000000000, 1.000000000000000000 ) ) ;
#3568 = CYLINDRICAL_SURFACE ( 'NONE', #10816, 9.000000000000000000 ) ;
#3569 = CARTESIAN_POINT ( 'NONE',  ( 23.77500000054622831, 20.00000000000000355, 98.07665518445361386 ) ) ;
#3570 = CARTESIAN_POINT ( 'NONE',  ( 27.57500000054622191, 26.19570976099943493, 95.29460816699764791 ) ) ;
#3571 = AXIS2_PLACEMENT_3D ( 'NONE', #1097, #209, #4425 ) ;
#3572 = DIRECTION ( 'NONE',  ( -0.000000000000000000, -0.000000000000000000, 1.000000000000000000 ) ) ;
#3573 = FACE_OUTER_BOUND ( 'NONE', #11963, .T. ) ;
#3574 = EDGE_LOOP ( 'NONE', ( #11222, #4512, #10657, #9534 ) ) ;
#3575 = CARTESIAN_POINT ( 'NONE',  ( 35.75000000109246656, 17.56310227825320425, 98.29316153445363113 ) ) ;
#3576 = CARTESIAN_POINT ( 'NONE',  ( 8.123360751522579193, 14.15902104166613107, 23.64419573351483450 ) ) ;
#3577 = VERTEX_POINT ( 'NONE', #2370 ) ;
#3578 = CARTESIAN_POINT ( 'NONE',  ( 0.000000000000000000, 22.00000000000000000, 169.9999999999999716 ) ) ;
#3579 = ADVANCED_FACE ( 'NONE', ( #12139 ), #9102, .F. ) ;
#3580 = EDGE_LOOP ( 'NONE', ( #12442, #5339, #6980, #7075 ) ) ;
#3581 = CARTESIAN_POINT ( 'NONE',  ( -4.146974088394097535, 10.89458658634673327, -24.65552811365946440 ) ) ;
#3582 = CARTESIAN_POINT ( 'NONE',  ( 31.65000000109246514, 20.00000000000000355, 98.29316153445363113 ) ) ;
#3583 = B_SPLINE_CURVE_WITH_KNOTS ( 'NONE', 3,
 ( #9070, #9195, #10082, #11090, #5324, #6210, #1267, #3167, #504, #7091, #8943, #9962, #4180, #10973, #380, #2281, #8057, #6149, #11986, #1393 ),
 .UNSPECIFIED., .F., .F.,
 ( 4, 2, 2, 2, 2, 2, 2, 2, 2, 4 ),
 ( 0.01567180661725443153, 0.01665134708417310289, 0.01763088755109177425, 0.01812065778455110993, 0.01861042801801044561, 0.01958996848492911697, 0.02056950895184778833, 0.02154904941876645622, 0.02252858988568512758, 0.02350813035260379893 ),
 .UNSPECIFIED. ) ;
#3584 = CARTESIAN_POINT ( 'NONE',  ( 20.47500000054622760, 13.80429023900056684, 86.29171490190961435 ) ) ;
#3585 = ADVANCED_FACE ( 'NONE', ( #9287 ), #7124, .F. ) ;
#3586 = CYLINDRICAL_SURFACE ( 'NONE', #318, 9.000000000000000000 ) ;
#3587 = CARTESIAN_POINT ( 'NONE',  ( 26.99999999999998934, 20.00000000000000355, 83.29316153445364534 ) ) ;
#3588 = CARTESIAN_POINT ( 'NONE',  ( 1.295434377910737567, 54.83206668271250805, -27.97046038954552216 ) ) ;
#3589 = DIRECTION ( 'NONE',  ( 0.000000000000000000, 1.000000000000000000, 0.000000000000000000 ) ) ;
#3590 = CARTESIAN_POINT ( 'NONE',  ( 21.47500000054622760, 26.19570976099943493, 95.29460816699764791 ) ) ;
#3591 = AXIS2_PLACEMENT_3D ( 'NONE', #4559, #2657, #5581 ) ;
#3592 = CARTESIAN_POINT ( 'NONE',  ( -2.000000000000015543, 20.00000000000000355, 90.79316153445363113 ) ) ;
#3593 = CARTESIAN_POINT ( 'NONE',  ( -4.331872009808981794, 52.50234731214368367, 24.62196273622729592 ) ) ;
#3594 = ORIENTED_EDGE ( 'NONE', *, *, #9449, .T. ) ;
#3595 = DIRECTION ( 'NONE',  ( -1.000000000000000000, -0.000000000000000000, -0.000000000000000000 ) ) ;
#3596 = FACE_OUTER_BOUND ( 'NONE', #10423, .T. ) ;
#3597 = CARTESIAN_POINT ( 'NONE',  ( 35.57500000054622546, 24.28113015263587116, 96.68563167572563088 ) ) ;
#3598 = CARTESIAN_POINT ( 'NONE',  ( 35.57500000054623257, 26.19570976099943493, 95.29460816699764791 ) ) ;
#3599 = CARTESIAN_POINT ( 'NONE',  ( 0.000000000000000000, 5.839897972853065333, -6.938893903907228378E-15 ) ) ;
#3600 = CARTESIAN_POINT ( 'NONE',  ( 4.999999999999997335, 22.00000000000000000, 152.2284161474004520 ) ) ;
#3601 = CARTESIAN_POINT ( 'NONE',  ( 0.6522419138580031195, 45.03179559853693092, 24.99358091562669060 ) ) ;
#3602 = CARTESIAN_POINT ( 'NONE',  ( 35.69999999999998153, 26.37988106264029398, 95.42841645007781892 ) ) ;
#3603 = DIRECTION ( 'NONE',  ( 0.000000000000000000, 0.4999999999999984457, -0.8660254037844394848 ) ) ;
#3604 = AXIS2_PLACEMENT_3D ( 'NONE', #9394, #10516, #7356 ) ;
#3605 = CARTESIAN_POINT ( 'NONE',  ( 3.061616997868383437E-15, -3.000000000000003109, -25.00000000000000355 ) ) ;
#3606 = EDGE_LOOP ( 'NONE', ( #11875, #10588, #7671, #10674, #11008 ) ) ;
#3607 = FACE_BOUND ( 'NONE', #11949, .T. ) ;
#3608 = CARTESIAN_POINT ( 'NONE',  ( 27.49999999999999645, 20.00000000000000355, 230.4654751958684642 ) ) ;
#3609 = AXIS2_PLACEMENT_3D ( 'NONE', #10825, #8933, #1258 ) ;
#3610 = DIRECTION ( 'NONE',  ( 0.000000000000000000, 0.000000000000000000, -1.000000000000000000 ) ) ;
#3611 = CARTESIAN_POINT ( 'NONE',  ( 47.97500000054622404, 15.71886984736413417, 96.68563167572563088 ) ) ;
#3612 = CARTESIAN_POINT ( 'NONE',  ( 27.97500000054622404, 17.63344945572769973, 98.07665518445361386 ) ) ;
#3613 = CARTESIAN_POINT ( 'NONE',  ( 27.29999999999998295, 26.37988106264029398, 86.15790661882942914 ) ) ;
#3614 = CARTESIAN_POINT ( 'NONE',  ( -50.00000000000001421, 40.00000000000000000, 69.99999999999998579 ) ) ;
#3615 = CARTESIAN_POINT ( 'NONE',  ( 36.37500000054622973, 13.07298590277314432, 88.54243821818161564 ) ) ;
#3616 = ORIENTED_EDGE ( 'NONE', *, *, #12033, .F. ) ;
#3617 = CARTESIAN_POINT ( 'NONE',  ( 20.65000000109246514, 20.00000000000000355, 83.29316153445364534 ) ) ;
#3618 = CARTESIAN_POINT ( 'NONE',  ( -5.000000000000000000, 50.00000000000000000, 20.39607805437114152 ) ) ;
#3619 = ORIENTED_EDGE ( 'NONE', *, *, #9086, .F. ) ;
#3620 = EDGE_CURVE ( 'NONE', #10817, #4738, #11985, .T. ) ;
#3621 = VECTOR ( 'NONE', #8505, 1000.000000000000114 ) ;
#3622 = CARTESIAN_POINT ( 'NONE',  ( -0.6666273477411399639, 30.00000000000001421, -28.00000000000000355 ) ) ;
#3623 = ORIENTED_EDGE ( 'NONE', *, *, #3361, .F. ) ;
#3624 = VECTOR ( 'NONE', #96, 1000.000000000000000 ) ;
#3625 =( NAMED_UNIT ( * ) SI_UNIT ( $, .STERADIAN. ) SOLID_ANGLE_UNIT ( ) );
#3626 = CARTESIAN_POINT ( 'NONE',  ( 21.65000000109246514, 20.00000000000000355, 98.29316153445363113 ) ) ;
#3627 = ADVANCED_FACE ( 'NONE', ( #11184 ), #468, .F. ) ;
#3628 = DIRECTION ( 'NONE',  ( 1.000000000000000000, 0.000000000000000000, 0.000000000000000000 ) ) ;
#3629 = CARTESIAN_POINT ( 'NONE',  ( 6.000000000000000000, 5.839897972853064445, -8.673617379884035472E-15 ) ) ;
#3630 = CARTESIAN_POINT ( 'NONE',  ( 27.17500000054622689, 26.92701409722686634, 88.54243821818162985 ) ) ;
#3631 = CARTESIAN_POINT ( 'NONE',  ( 49.79999999999999005, 24.40838939219354842, 96.86078899226572503 ) ) ;
#3632 = LINE ( 'NONE', #4713, #899 ) ;
#3633 = DIRECTION ( 'NONE',  ( -1.000000000000000000, -0.000000000000000000, -0.000000000000000000 ) ) ;
#3634 = VERTEX_POINT ( 'NONE', #10114 ) ;
#3635 = CARTESIAN_POINT ( 'NONE',  ( 39.25000000109246656, 27.13292387221364876, 93.11078899226573924 ) ) ;
#3636 = CARTESIAN_POINT ( 'NONE',  ( 24.09999999999998366, 17.56310227825320425, 98.29316153445363113 ) ) ;
#3637 = ORIENTED_EDGE ( 'NONE', *, *, #2298, .F. ) ;
#3638 = CARTESIAN_POINT ( 'NONE',  ( 27.49999999999999645, 20.00000000000000355, 188.9999999999999716 ) ) ;
#3639 = EDGE_LOOP ( 'NONE', ( #921, #9880, #2866, #836 ) ) ;
#3640 = CIRCLE ( 'NONE', #10729, 10.00000000000000355 ) ;
#3641 = CARTESIAN_POINT ( 'NONE',  ( -1.002883791299520887E-19, 10.00000000000000000, -25.00000000000000000 ) ) ;
#3642 = EDGE_CURVE ( 'NONE', #8125, #8822, #3658, .T. ) ;
#3643 = CARTESIAN_POINT ( 'NONE',  ( -0.6569842770428546697, 54.96739046863824996, -24.99342020365237360 ) ) ;
#3644 = DIRECTION ( 'NONE',  ( -0.5000000000000046629, 0.000000000000000000, 0.8660254037844359321 ) ) ;
#3645 = EDGE_CURVE ( 'NONE', #6159, #10270, #2221, .T. ) ;
#3646 = DIRECTION ( 'NONE',  ( 0.000000000000000000, 0.000000000000000000, 1.000000000000000000 ) ) ;
#3647 = ORIENTED_EDGE ( 'NONE', *, *, #6068, .F. ) ;
#3648 = TOROIDAL_SURFACE ( 'NONE', #8135, 5.400000000000001243, 0.4000000000000000222 ) ;
#3649 = CARTESIAN_POINT ( 'NONE',  ( 3.306945158608051827, 53.76431800115727100, -27.80499802709851664 ) ) ;
#3650 = DIRECTION ( 'NONE',  ( 0.000000000000000000, 0.000000000000000000, -1.000000000000000000 ) ) ;
#3651 = CARTESIAN_POINT ( 'NONE',  ( 20.67500000054622333, 17.63344945572770328, 83.50966788445364841 ) ) ;
#3652 = DIRECTION ( 'NONE',  ( 0.000000000000000000, 0.000000000000000000, -1.000000000000000000 ) ) ;
#3653 = CARTESIAN_POINT ( 'NONE',  ( 6.000000000000000000, -5.839897972853063557, 6.938893903907228378E-15 ) ) ;
#3654 = ORIENTED_EDGE ( 'NONE', *, *, #11082, .F. ) ;
#3656 = ADVANCED_FACE ( 'NONE', ( #6422 ), #8269, .T. ) ;
#3655 =( BOUNDED_CURVE ( )  B_SPLINE_CURVE ( 3, ( #294, #7430, #7304, #7365 ),
 .UNSPECIFIED., .F., .F. ) 
 B_SPLINE_CURVE_WITH_KNOTS ( ( 4, 4 ),
 ( 3.141592653589793560, 4.712388980384689674 ),
 .UNSPECIFIED. ) 
 CURVE ( )  GEOMETRIC_REPRESENTATION_ITEM ( )  RATIONAL_B_SPLINE_CURVE ( ( 1.000000000000000000, 0.8047378541243650485, 0.8047378541243650485, 1.000000000000000000 ) ) 
 REPRESENTATION_ITEM ( '' )  );
#3657 = ORIENTED_EDGE ( 'NONE', *, *, #4358, .T. ) ;
#3658 = CIRCLE ( 'NONE', #6307, 21.00000000000000000 ) ;
#3659 = CARTESIAN_POINT ( 'NONE',  ( -9.657265040632822206, 22.61657440465215174, -18.64803156764659775 ) ) ;
#3660 = DIRECTION ( 'NONE',  ( 0.000000000000000000, -0.000000000000000000, 1.000000000000000000 ) ) ;
#3661 = CARTESIAN_POINT ( 'NONE',  ( 38.77500000054622831, 17.63344945572770328, 83.50966788445364841 ) ) ;
#3662 = EDGE_CURVE ( 'NONE', #5412, #10229, #557, .T. ) ;
#3663 = CARTESIAN_POINT ( 'NONE',  ( 22.67500000054622333, 17.63344945572770328, 83.50966788445364841 ) ) ;
#3664 = CARTESIAN_POINT ( 'NONE',  ( 36.99999999999999289, 20.00000000000000355, 188.9999999999999716 ) ) ;
#3665 = DIRECTION ( 'NONE',  ( 0.000000000000000000, -1.000000000000000000, -0.000000000000000000 ) ) ;
#3666 = APPLICATION_CONTEXT ( 'automotive_design' ) ;
#3667 = FACE_OUTER_BOUND ( 'NONE', #7123, .T. ) ;
#3668 = CARTESIAN_POINT ( 'NONE',  ( 3.053082855025198494, 46.02690843307048141, -20.77868449535670692 ) ) ;
#3669 = CARTESIAN_POINT ( 'NONE',  ( 8.919948986426568638, 0.000000000000000000, 0.000000000000000000 ) ) ;
#3670 = ORIENTED_EDGE ( 'NONE', *, *, #10391, .F. ) ;
#3671 = CARTESIAN_POINT ( 'NONE',  ( 31.00470515163597085, 12.50000000000001243, 148.5047051516359602 ) ) ;
#3672 =( NAMED_UNIT ( * ) PLANE_ANGLE_UNIT ( ) SI_UNIT ( $, .RADIAN. ) );
#3673 = CARTESIAN_POINT ( 'NONE',  ( 25.87500000054622618, 20.00000000000000355, 98.07665518445361386 ) ) ;
#3674 = CARTESIAN_POINT ( 'NONE',  ( 29.55000000109246727, 22.43689772174679575, 98.29316153445363113 ) ) ;
#3675 = CARTESIAN_POINT ( 'NONE',  ( 39.87500000054622262, 17.63344945572769973, 98.07665518445361386 ) ) ;
#3676 = CARTESIAN_POINT ( 'NONE',  ( 26.97500000054622049, 22.36655054427230382, 83.50966788445364841 ) ) ;
#3677 = CARTESIAN_POINT ( 'NONE',  ( 28.79999999999999005, 15.59161060780646046, 84.72553407664153724 ) ) ;
#3678 = CARTESIAN_POINT ( 'NONE',  ( 0.000000000000000000, 50.00000000000000000, -28.00000000000000711 ) ) ;
#3679 = CARTESIAN_POINT ( 'NONE',  ( 36.97500000054623115, 24.28113015263587471, 84.90069139318163138 ) ) ;
#3680 = EDGE_LOOP ( 'NONE', ( #12031, #12477 ) ) ;
#3681 = CARTESIAN_POINT ( 'NONE',  ( 48.57500000054623257, 15.71886984736413773, 84.90069139318163138 ) ) ;
#3682 = DIRECTION ( 'NONE',  ( -0.000000000000000000, -1.000000000000000000, -0.000000000000000000 ) ) ;
#3683 = EDGE_LOOP ( 'NONE', ( #2378, #5121, #10130, #9205, #9519, #395 ) ) ;
#3684 = CARTESIAN_POINT ( 'NONE',  ( 5.000000000000000000, 50.00000000000000000, 27.54995462791182703 ) ) ;
#3685 = EDGE_LOOP ( 'NONE', ( #4549, #30 ) ) ;
#3686 = CARTESIAN_POINT ( 'NONE',  ( -1.297374591076399408, 54.83977433137422253, -24.96837001061641104 ) ) ;
#3687 = CARTESIAN_POINT ( 'NONE',  ( 4.999999999999999112, -3.000000000000002665, 218.7511230907454944 ) ) ;
#3688 = CARTESIAN_POINT ( 'NONE',  ( 43.37500000054622973, 27.65831843345427998, 90.79316153445363113 ) ) ;
#3689 = FACE_OUTER_BOUND ( 'NONE', #9207, .T. ) ;
#3690 = EDGE_CURVE ( 'NONE', #11695, #3276, #7626, .T. ) ;
#3691 = CARTESIAN_POINT ( 'NONE',  ( 43.37500000054622973, 27.65831843345427998, 90.79316153445363113 ) ) ;
#3692 = CARTESIAN_POINT ( 'NONE',  ( 49.49999999999998579, 27.88596668178699645, 90.79316153445363113 ) ) ;
#3693 = DIRECTION ( 'NONE',  ( 1.000000000000000000, 0.000000000000000000, 0.000000000000000000 ) ) ;
#3694 = CARTESIAN_POINT ( 'NONE',  ( 38.85000000109246798, 24.40838939219355197, 84.72553407664153724 ) ) ;
#3695 = ORIENTED_EDGE ( 'NONE', *, *, #6971, .F. ) ;
#3696 = AXIS2_PLACEMENT_3D ( 'NONE', #8258, #8137, #10164 ) ;
#3697 = CARTESIAN_POINT ( 'NONE',  ( 40.45000000109246940, 15.59161060780646046, 84.72553407664153724 ) ) ;
#3698 = CARTESIAN_POINT ( 'NONE',  ( 24.49999999999998579, 12.11403331821300533, 90.79316153445363113 ) ) ;
#3699 = VERTEX_POINT ( 'NONE', #4770 ) ;
#3700 = CARTESIAN_POINT ( 'NONE',  ( 12.00000000000000000, 0.000000000000000000, -6.599999999999999645 ) ) ;
#3701 = EDGE_LOOP ( 'NONE', ( #1143, #7125, #4972, #3499, #7374 ) ) ;
#3702 = PLANE ( 'NONE',  #9711 ) ;
#3703 = CARTESIAN_POINT ( 'NONE',  ( 31.35000000109246088, 26.37988106264029398, 95.42841645007781892 ) ) ;
#3704 = PLANE ( 'NONE',  #7398 ) ;
#3705 = CARTESIAN_POINT ( 'NONE',  ( -4.493239192008157801, 47.78244187540930454, 20.51407495533472414 ) ) ;
#3706 = ORIENTED_EDGE ( 'NONE', *, *, #7422, .F. ) ;
#3707 = EDGE_CURVE ( 'NONE', #11366, #5684, #8575, .T. ) ;
#3708 = LINE ( 'NONE', #7591, #9421 ) ;
#3709 = CARTESIAN_POINT ( 'NONE',  ( 12.59999999999999964, 0.000000000000000000, 0.000000000000000000 ) ) ;
#3710 = CARTESIAN_POINT ( 'NONE',  ( 22.77500000054622831, 20.00000000000000355, 83.50966788445364841 ) ) ;
#3711 = CARTESIAN_POINT ( 'NONE',  ( 45.85000000109246798, 15.59161060780645691, 96.86078899226572503 ) ) ;
#3712 = VECTOR ( 'NONE', #10492, 1000.000000000000114 ) ;
#3713 = CARTESIAN_POINT ( 'NONE',  ( 5.000000000000000000, 4.685197434473814759, -5.637851296924623057E-15 ) ) ;
#3714 = VERTEX_POINT ( 'NONE', #5543 ) ;
#3715 = ORIENTED_EDGE ( 'NONE', *, *, #3186, .T. ) ;
#3716 = CARTESIAN_POINT ( 'NONE',  ( 21.09999999999998366, 22.43689772174679575, 83.29316153445363113 ) ) ;
#3717 = FACE_OUTER_BOUND ( 'NONE', #7893, .T. ) ;
#3718 = VECTOR ( 'NONE', #1787, 1000.000000000000000 ) ;
#3719 = DIRECTION ( 'NONE',  ( 0.000000000000000000, 0.000000000000000000, 1.000000000000000000 ) ) ;
#3720 = DIRECTION ( 'NONE',  ( 0.000000000000000000, 0.000000000000000000, -1.000000000000000000 ) ) ;
#3721 = TOROIDAL_SURFACE ( 'NONE', #10818, 17.49999999999996803, 10.00000000000000000 ) ;
#3722 = ADVANCED_FACE ( 'NONE', ( #10469 ), #6482, .T. ) ;
#3723 = DIRECTION ( 'NONE',  ( -1.000000000000000000, 0.000000000000000000, 0.000000000000000000 ) ) ;
#3724 = DIRECTION ( 'NONE',  ( 1.000000000000000000, -0.000000000000000000, -0.000000000000000000 ) ) ;
#3725 =( BOUNDED_CURVE ( )  B_SPLINE_CURVE ( 2, ( #8990, #107, #7904, #8983, #2059, #2125, #3078, #6943, #7968, #8916, #1124, #297, #4989, #41, #8849, #11773, #4092, #11836, #2196, #6067, #5118, #9939, #1247, #1972, #972, #10539, #5731, #10596, #5606, #1848, #12512, #5856, #9725, #9598, #906, #12451, #8518, #1042, #4902, #11436, #2869, #6669, #8762, #6796, #3943, #1908, #4776, #4840, #8641, #3817, #3751, #6729, #10474, #5671, #5793, #2932, #7568, #80, #9664, #10661, #1786, #11376, #16, #3879, #2682, #3688, #7753, #6547, #6605, #11624, #10414, #1728, #9479, #779, #2747, #4647, #12391, #9541, #840, #4708, #8580, #7633, #11496, #2804, #10724, #7047, #8959, #10787, #7880, #5030, #273, #8894, #4135, #9089, #11750, #8008, #2099, #1286, #7113, #4068, #4200, #397, #6920, #11880, #10925, #2239, #337, #6107, #210, #7819, #6987, #11688, #3246, #2994, #9976, #10858, #5219, #146, #6861, #5159, #10042, #10988, #9026, #2168, #6040, #8075, #2037, #11942, #5917, #9851, #11812, #9786, #2296, #6168, #1098, #9915, #4964, #1165, #1353, #8826, #4003, #5976, #3058, #7946, #1225, #5093, #3305, #10333, #6350, #5472, #12248, #8136, #10218, #4504, #7173, #6228, #1530, #5532, #3367, #8322, #5404, #9275, #1414, #8379, #9152, #5342, #5281, #7237, #11050, #3435, #9338, #7297, #11110, #641, #11171, #3551, #1469, #7425, #6411, #2475, #579, #9213, #10273, #9396, #519, #6291, #2358, #2415, #4445, #12127, #12003, #11295, #12189, #3489, #11228, #7360, #4380, #10163, #2538, #1590, #2600, #6471, #1650, #4259, #10101, #8257, #458, #4320, #8197, #12067, #1831, #3863, #7739, #12434, #2787, #1766, #1709, #11605, #6778, #4630, #4757, #6649, #5836, #8689, #700, #12493, #10518, #6714, #5714, #9580, #5650, #887, #12373, #7550, #8623, #1298, #9461, #4567, #11542, #8440, #3673, #12309, #9647, #7676, #7487, #5590, #2851, #11358, #8500, #955, #2666, #6527, #11419, #2729, #10456, #9523, #821, #2019, #7802, #3232, #5011, #4946, #8945, #4182, #10708, #9898, #6025, #1212, #61, #9770, #5078, #7033, #4114, #7093, #11674, #10839, #8058, #9963, #7993, #11925, #257, #11862, #8875, #4050, #3169, #3927, #10907, #4884, #11736, #1148, #9708, #2222, #2152, #1024, #193, #2981, #3040, #1270, #10974, #6845, #320 ),
 .UNSPECIFIED., .F., .F. ) 
 B_SPLINE_CURVE_WITH_KNOTS ( ( 3, 2, 2, 2, 2, 2, 2, 2, 2, 2, 2, 2, 2, 2, 2, 2, 2, 2, 2, 2, 2, 2, 2, 2, 2, 2, 2, 2, 2, 2, 2, 2, 2, 2, 2, 2, 2, 2, 2, 2, 2, 2, 2, 2, 2, 2, 2, 2, 2, 2, 2, 2, 2, 2, 2, 2, 2, 2, 2, 2, 2, 2, 2, 2, 2, 2, 2, 2, 2, 2, 2, 2, 2, 2, 2, 2, 2, 2, 2, 2, 2, 2, 2, 2, 2, 2, 2, 2, 2, 2, 2, 2, 2, 2, 2, 2, 2, 2, 2, 2, 2, 2, 2, 2, 2, 2, 2, 2, 2, 2, 2, 2, 2, 2, 2, 2, 2, 2, 2, 2, 2, 2, 2, 2, 2, 2, 2, 2, 2, 2, 2, 2, 2, 2, 2, 2, 2, 2, 2, 2, 2, 2, 2, 2, 2, 2, 2, 2, 2, 2, 3 ),
 ( 0.000000000000000000, 0.006666666666666667095, 0.01333333333333333419, 0.02000000000000000042, 0.02666666666666666838, 0.03333333333333333287, 0.04000000000000000083, 0.04666666666666666879, 0.05333333333333333676, 0.05999999999999999778, 0.06666666666666666574, 0.07333333333333333370, 0.08000000000000000167, 0.08666666666666666963, 0.09333333333333333759, 0.1000000000000000056, 0.1066666666666666735, 0.1133333333333333276, 0.1199999999999999956, 0.1266666666666666774, 0.1333333333333333315, 0.1400000000000000133, 0.1466666666666666674, 0.1533333333333333215, 0.1600000000000000033, 0.1666666666666666574, 0.1733333333333333393, 0.1799999999999999933, 0.1866666666666666752, 0.1933333333333333293, 0.2000000000000000111, 0.2066666666666666652, 0.2133333333333333470, 0.2200000000000000011, 0.2266666666666666552, 0.2333333333333333370, 0.2399999999999999911, 0.2466666666666666730, 0.2533333333333333548, 0.2600000000000000089, 0.2666666666666666630, 0.2733333333333333171, 0.2800000000000000266, 0.2866666666666666807, 0.2933333333333333348, 0.2999999999999999889, 0.3066666666666666430, 0.3133333333333333526, 0.3200000000000000067, 0.3266666666666666607, 0.3333333333333333148, 0.3400000000000000244, 0.3466666666666666785, 0.3533333333333333326, 0.3599999999999999867, 0.3666666666666666408, 0.3733333333333333504, 0.3800000000000000044, 0.3866666666666666585, 0.3933333333333333126, 0.4000000000000000222, 0.4066666666666666763, 0.4133333333333333304, 0.4199999999999999845, 0.4266666666666666941, 0.4333333333333333481, 0.4400000000000000022, 0.4466666666666666563, 0.4533333333333333104, 0.4600000000000000200, 0.4666666666666666741, 0.4733333333333333282, 0.4799999999999999822, 0.4866666666666666918, 0.4933333333333333459, 0.5000000000000000000, 0.5066666666666667096, 0.5133333333333333082, 0.5200000000000000178, 0.5266666666666666163, 0.5333333333333333259, 0.5400000000000000355, 0.5466666666666666341, 0.5533333333333333437, 0.5600000000000000533, 0.5666666666666666519, 0.5733333333333333615, 0.5799999999999999600, 0.5866666666666666696, 0.5933333333333333792, 0.5999999999999999778, 0.6066666666666666874, 0.6133333333333332860, 0.6199999999999999956, 0.6266666666666667052, 0.6333333333333333037, 0.6400000000000000133, 0.6466666666666666119, 0.6533333333333333215, 0.6600000000000000311, 0.6666666666666666297, 0.6733333333333333393, 0.6800000000000000488, 0.6866666666666666474, 0.6933333333333333570, 0.6999999999999999556, 0.7066666666666666652, 0.7133333333333333748, 0.7199999999999999734, 0.7266666666666666829, 0.7333333333333332815, 0.7399999999999999911, 0.7466666666666667007, 0.7533333333333332993, 0.7600000000000000089, 0.7666666666666667185, 0.7733333333333333171, 0.7800000000000000266, 0.7866666666666666252, 0.7933333333333333348, 0.8000000000000000444, 0.8066666666666666430, 0.8133333333333333526, 0.8199999999999999512, 0.8266666666666666607, 0.8333333333333333703, 0.8399999999999999689, 0.8466666666666666785, 0.8533333333333333881, 0.8599999999999999867, 0.8666666666666666963, 0.8733333333333332948, 0.8800000000000000044, 0.8866666666666667140, 0.8933333333333333126, 0.9000000000000000222, 0.9066666666666666208, 0.9133333333333333304, 0.9200000000000000400, 0.9266666666666666385, 0.9333333333333333481, 0.9399999999999999467, 0.9466666666666666563, 0.9533333333333333659, 0.9599999999999999645, 0.9666666666666666741, 0.9733333333333333837, 0.9799999999999999822, 0.9866666666666666918, 0.9933333333333332904, 1.000000000000000000 ),
 .UNSPECIFIED. ) 
 CURVE ( )  GEOMETRIC_REPRESENTATION_ITEM ( )  RATIONAL_B_SPLINE_CURVE ( ( 1.000000000000000000, 0.9510565162951535312, 1.000000000000000000, 0.9510565162951535312, 1.000000000000000000, 0.9510565162951535312, 1.000000000000000000, 0.9510565162951535312, 1.000000000000000000, 0.9510565162951535312, 1.000000000000000000, 0.9510565162951535312, 1.000000000000000000, 0.9510565162951535312, 1.000000000000000000, 0.9510565162951535312, 1.000000000000000000, 0.9510565162951535312, 1.000000000000000000, 0.9510565162951535312, 1.000000000000000000, 0.9510565162951535312, 1.000000000000000000, 0.9510565162951535312, 1.000000000000000000, 0.9510565162951535312, 1.000000000000000000, 0.9510565162951535312, 1.000000000000000000, 0.9510565162951535312, 1.000000000000000000, 0.9510565162951535312, 1.000000000000000000, 0.9510565162951535312, 1.000000000000000000, 0.9510565162951535312, 1.000000000000000000, 0.9510565162951535312, 1.000000000000000000, 0.9510565162951535312, 1.000000000000000000, 0.9510565162951535312, 1.000000000000000000, 0.9510565162951535312, 1.000000000000000000, 0.9510565162951535312, 1.000000000000000000, 0.9510565162951535312, 1.000000000000000000, 0.9510565162951535312, 1.000000000000000000, 0.9510565162951535312, 1.000000000000000000, 0.9510565162951535312, 1.000000000000000000, 0.9510565162951535312, 1.000000000000000000, 0.9510565162951535312, 1.000000000000000000, 0.9510565162951535312, 1.000000000000000000, 0.9510565162951535312, 1.000000000000000000, 0.9510565162951535312, 1.000000000000000000, 0.9510565162951535312, 1.000000000000000000, 0.9510565162951535312, 1.000000000000000000, 0.9510565162951535312, 1.000000000000000000, 0.9510565162951535312, 1.000000000000000000, 0.9510565162951535312, 1.000000000000000000, 0.9510565162951535312, 1.000000000000000000, 0.9510565162951535312, 1.000000000000000000, 0.9510565162951535312, 1.000000000000000000, 0.9510565162951535312, 1.000000000000000000, 0.9510565162951535312, 1.000000000000000000, 0.9510565162951535312, 1.000000000000000000, 0.9510565162951535312, 1.000000000000000000, 0.9510565162951535312, 1.000000000000000000, 0.9510565162951535312, 1.000000000000000000, 0.9510565162951535312, 1.000000000000000000, 0.9510565162951535312, 1.000000000000000000, 0.9510565162951535312, 1.000000000000000000, 0.9510565162951535312, 1.000000000000000000, 0.9510565162951535312, 1.000000000000000000, 0.9510565162951535312, 1.000000000000000000, 0.9510565162951535312, 1.000000000000000000, 0.9510565162951535312, 1.000000000000000000, 0.9510565162951535312, 1.000000000000000000, 0.9510565162951535312, 1.000000000000000000, 0.9510565162951535312, 1.000000000000000000, 0.9510565162951535312, 1.000000000000000000, 0.9510565162951535312, 1.000000000000000000, 0.9510565162951535312, 1.000000000000000000, 0.9510565162951535312, 1.000000000000000000, 0.9510565162951535312, 1.000000000000000000, 0.9510565162951535312, 1.000000000000000000, 0.9510565162951535312, 1.000000000000000000, 0.9510565162951535312, 1.000000000000000000, 0.9510565162951535312, 1.000000000000000000, 0.9510565162951535312, 1.000000000000000000, 0.9510565162951535312, 1.000000000000000000, 0.9510565162951535312, 1.000000000000000000, 0.9510565162951535312, 1.000000000000000000, 0.9510565162951535312, 1.000000000000000000, 0.9510565162951535312, 1.000000000000000000, 0.9510565162951535312, 1.000000000000000000, 0.9510565162951535312, 1.000000000000000000, 0.9510565162951535312, 1.000000000000000000, 0.9510565162951535312, 1.000000000000000000, 0.9510565162951535312, 1.000000000000000000, 0.9510565162951535312, 1.000000000000000000, 0.9510565162951535312, 1.000000000000000000, 0.9510565162951535312, 1.000000000000000000, 0.9510565162951535312, 1.000000000000000000, 0.9510565162951535312, 1.000000000000000000, 0.9510565162951535312, 1.000000000000000000, 0.9510565162951535312, 1.000000000000000000, 0.9510565162951535312, 1.000000000000000000, 0.9510565162951535312, 1.000000000000000000, 0.9510565162951535312, 1.000000000000000000, 0.9510565162951535312, 1.000000000000000000, 0.9510565162951535312, 1.000000000000000000, 0.9510565162951535312, 1.000000000000000000, 0.9510565162951535312, 1.000000000000000000, 0.9510565162951535312, 1.000000000000000000, 0.9510565162951535312, 1.000000000000000000, 0.9510565162951535312, 1.000000000000000000, 0.9510565162951535312, 1.000000000000000000, 0.9510565162951535312, 1.000000000000000000, 0.9510565162951535312, 1.000000000000000000, 0.9510565162951535312, 1.000000000000000000, 0.9510565162951535312, 1.000000000000000000, 0.9510565162951535312, 1.000000000000000000, 0.9510565162951535312, 1.000000000000000000, 0.9510565162951535312, 1.000000000000000000, 0.9510565162951535312, 1.000000000000000000, 0.9510565162951535312, 1.000000000000000000, 0.9510565162951535312, 1.000000000000000000, 0.9510565162951535312, 1.000000000000000000, 0.9510565162951535312, 1.000000000000000000, 0.9510565162951535312, 1.000000000000000000, 0.9510565162951535312, 1.000000000000000000, 0.9510565162951535312, 1.000000000000000000, 0.9510565162951535312, 1.000000000000000000, 0.9510565162951535312, 1.000000000000000000, 0.9510565162951535312, 1.000000000000000000, 0.9510565162951535312, 1.000000000000000000, 0.9510565162951535312, 1.000000000000000000, 0.9510565162951535312, 1.000000000000000000, 0.9510565162951535312, 1.000000000000000000, 0.9510565162951535312, 1.000000000000000000, 0.9510565162951535312, 1.000000000000000000, 0.9510565162951535312, 1.000000000000000000, 0.9510565162951535312, 1.000000000000000000, 0.9510565162951535312, 1.000000000000000000, 0.9510565162951535312, 1.000000000000000000, 0.9510565162951535312, 1.000000000000000000, 0.9510565162951535312, 1.000000000000000000, 0.9510565162951535312, 1.000000000000000000, 0.9510565162951535312, 1.000000000000000000, 0.9510565162951535312, 1.000000000000000000, 0.9510565162951535312, 1.000000000000000000, 0.9510565162951535312, 1.000000000000000000, 0.9510565162951535312, 1.000000000000000000, 0.9510565162951535312, 1.000000000000000000, 0.9510565162951535312, 1.000000000000000000, 0.9510565162951535312, 1.000000000000000000, 0.9510565162951535312, 1.000000000000000000, 0.9510565162951535312, 1.000000000000000000, 0.9510565162951535312, 1.000000000000000000, 0.9510565162951535312, 1.000000000000000000, 0.9510565162951535312, 1.000000000000000000, 0.9510565162951535312, 1.000000000000000000, 0.9510565162951535312, 1.000000000000000000, 0.9510565162951535312, 1.000000000000000000, 0.9510565162951535312, 1.000000000000000000, 0.9510565162951535312, 1.000000000000000000, 0.9510565162951535312, 1.000000000000000000, 0.9510565162951535312, 1.000000000000000000, 0.9510565162951535312, 1.000000000000000000, 0.9510565162951535312, 1.000000000000000000, 0.9510565162951535312, 1.000000000000000000, 0.9510565162951535312, 1.000000000000000000 ) ) 
 REPRESENTATION_ITEM ( '' )  );
#3726 = LINE ( 'NONE', #11536, #1340 ) ;
#3727 = DIRECTION ( 'NONE',  ( 8.659560562354932858E-17, 0.7071067811865474617, -0.7071067811865474617 ) ) ;
#3728 = ORIENTED_EDGE ( 'NONE', *, *, #9717, .T. ) ;
#3729 = CARTESIAN_POINT ( 'NONE',  ( 49.99999999999998579, 22.00000000000000000, 152.2284161474004520 ) ) ;
#3730 = EDGE_CURVE ( 'NONE', #5701, #7957, #9795, .T. ) ;
#3731 = AXIS2_PLACEMENT_3D ( 'NONE', #9126, #11085, #2390 ) ;
#3732 = B_SPLINE_CURVE_WITH_KNOTS ( 'NONE', 3,
 ( #1993, #231, #1059, #8913, #5874, #4922, #104, #6940, #3964, #7965, #11833, #5409, #12132, #3440, #12254, #3494, #10223, #705, #11177, #5477, #6476, #9344, #10402, #9403, #646, #8980, #8031, #8446 ),
 .UNSPECIFIED., .F., .F.,
 ( 4, 2, 2, 2, 2, 2, 2, 2, 2, 2, 2, 2, 2, 4 ),
 ( 0.03175036704783668062, 0.03274152275842889814, 0.03373267846902110872, 0.03571498989020553683, 0.03670614560079775435, 0.03769730131138997187, 0.03868845702198218245, 0.03967961273257439997, 0.04166192415375883501, 0.04265307986435105253, 0.04364423557494327005, 0.04562654699612770509, 0.04661770270671992261, 0.04760885841731214013 ),
 .UNSPECIFIED. ) ;
#3733 = CARTESIAN_POINT ( 'NONE',  ( 28.65000000109246514, 20.00000000000000355, 83.29316153445364534 ) ) ;
#3734 = CARTESIAN_POINT ( 'NONE',  ( 42.57500000054623257, 15.71886984736413773, 84.90069139318163138 ) ) ;
#3735 = ADVANCED_FACE ( 'NONE', ( #5602 ), #3868, .T. ) ;
#3736 = CARTESIAN_POINT ( 'NONE',  ( 30.17500000054621978, 13.80429023900056507, 95.29460816699764791 ) ) ;
#3737 = CARTESIAN_POINT ( 'NONE',  ( 27.89999999999998792, 22.43689772174679575, 98.29316153445363113 ) ) ;
#3738 =( NAMED_UNIT ( * ) PLANE_ANGLE_UNIT ( ) SI_UNIT ( $, .RADIAN. ) );
#3739 = CARTESIAN_POINT ( 'NONE',  ( 39.27500000054622120, 27.65831843345427998, 90.79316153445363113 ) ) ;
#3740 = VERTEX_POINT ( 'NONE', #12386 ) ;
#3741 =( GEOMETRIC_REPRESENTATION_CONTEXT ( 3 ) GLOBAL_UNCERTAINTY_ASSIGNED_CONTEXT ( ( #1001 ) ) GLOBAL_UNIT_ASSIGNED_CONTEXT ( ( #909, #4778, #8708 ) ) REPRESENTATION_CONTEXT ( 'NONE', 'WORKASPACE' ) );
#3742 = CARTESIAN_POINT ( 'NONE',  ( 20.35000000109246088, 13.62011893735971135, 86.15790661882942914 ) ) ;
#3743 = CARTESIAN_POINT ( 'NONE',  ( -31.74999999999995737, 0.000000000000000000, 0.000000000000000000 ) ) ;
#3744 = ORIENTED_EDGE ( 'NONE', *, *, #1029, .T. ) ;
#3745 = CARTESIAN_POINT ( 'NONE',  ( 6.000000000000000000, 0.000000000000000000, 5.057500000000000107 ) ) ;
#3746 = ORIENTED_EDGE ( 'NONE', *, *, #4038, .T. ) ;
#3747 = CARTESIAN_POINT ( 'NONE',  ( 9.104442389086463194, 24.14915179589751304, -23.28362858151144721 ) ) ;
#3748 = CARTESIAN_POINT ( 'NONE',  ( 32.89999999999998437, 17.56310227825320425, 83.29316153445363113 ) ) ;
#3749 = VECTOR ( 'NONE', #11748, 1000.000000000000000 ) ;
#3750 = LINE ( 'NONE', #11495, #2184 ) ;
#3751 = CARTESIAN_POINT ( 'NONE',  ( 44.87500000054622973, 20.00000000000000355, 83.50966788445364841 ) ) ;
#3752 = DIRECTION ( 'NONE',  ( -0.000000000000000000, -0.000000000000000000, -1.000000000000000000 ) ) ;
#3753 = AXIS2_PLACEMENT_3D ( 'NONE', #5880, #2896, #3652 ) ;
#3754 = DIRECTION ( 'NONE',  ( 1.000000000000000000, -0.000000000000000000, -0.000000000000000000 ) ) ;
#3755 = CARTESIAN_POINT ( 'NONE',  ( 42.87500000054622262, 20.00000000000000355, 83.50966788445364841 ) ) ;
#3756 = CARTESIAN_POINT ( 'NONE',  ( 45.79999999999999005, 24.40838939219354842, 96.86078899226572503 ) ) ;
#3757 = CARTESIAN_POINT ( 'NONE',  ( -0.6685289520415670372, 30.00000000000001776, -25.00000000000001066 ) ) ;
#3758 = CARTESIAN_POINT ( 'NONE',  ( 38.75000000109247367, 22.43689772174678509, 83.29316153445363113 ) ) ;
#3759 = ORIENTED_EDGE ( 'NONE', *, *, #6426, .T. ) ;
#3760 = CARTESIAN_POINT ( 'NONE',  ( 40.85000000109246088, 24.40838939219355197, 84.72553407664153724 ) ) ;
#3761 = FILL_AREA_STYLE_COLOUR ( '', #1032 ) ;
#3762 = FACE_OUTER_BOUND ( 'NONE', #3606, .T. ) ;
#3763 = EDGE_LOOP ( 'NONE', ( #6541, #10187, #8423, #3545 ) ) ;
#3764 = AXIS2_PLACEMENT_3D ( 'NONE', #11012, #9878, #5122 ) ;
#3765 = EDGE_CURVE ( 'NONE', #5573, #6725, #10838, .T. ) ;
#3766 = CARTESIAN_POINT ( 'NONE',  ( -1.002883791299520887E-19, 10.00000000000000000, -25.00000000000000000 ) ) ;
#3767 = CARTESIAN_POINT ( 'NONE',  ( 31.45000000109246585, 24.40838939219354842, 96.86078899226572503 ) ) ;
#3768 = CARTESIAN_POINT ( 'NONE',  ( 6.000000000000000000, 5.258101095580058680E-15, 5.057500000000000107 ) ) ;
#3769 = EDGE_CURVE ( 'NONE', #174, #2354, #11617, .T. ) ;
#3770 = FACE_OUTER_BOUND ( 'NONE', #6842, .T. ) ;
#3771 = CARTESIAN_POINT ( 'NONE',  ( -4.838567600861090057, 48.69772713945680209, 20.43508361496535031 ) ) ;
#3772 = VERTEX_POINT ( 'NONE', #8888 ) ;
#3773 = DIRECTION ( 'NONE',  ( -1.000000000000000000, -0.000000000000000000, -0.000000000000000000 ) ) ;
#3774 = CARTESIAN_POINT ( 'NONE',  ( 50.99999999999999289, 20.00000000000000711, 189.9999999999999716 ) ) ;
#3775 = CARTESIAN_POINT ( 'NONE',  ( 21.77500000054622831, 20.00000000000000355, 98.07665518445361386 ) ) ;
#3776 = ORIENTED_EDGE ( 'NONE', *, *, #8676, .F. ) ;
#3777 = FACE_OUTER_BOUND ( 'NONE', #93, .T. ) ;
#3778 = PLANE ( 'NONE',  #7112 ) ;
#3779 = ORIENTED_EDGE ( 'NONE', *, *, #11307, .T. ) ;
#3780 = VECTOR ( 'NONE', #4999, 999.9999999999998863 ) ;
#3781 = ORIENTED_EDGE ( 'NONE', *, *, #7695, .T. ) ;
#3782 = CARTESIAN_POINT ( 'NONE',  ( -7.523626141222965025, 26.59539293290133344, -19.60723250985141775 ) ) ;
#3783 = ADVANCED_FACE ( 'NONE', ( #10854 ), #4479, .T. ) ;
#3784 = LINE ( 'NONE', #12360, #9881 ) ;
#3785 =( BOUNDED_CURVE ( )  B_SPLINE_CURVE ( 2, ( #3626, #8273, #2618, #6241, #10118, #6368, #1606, #6425, #1428, #5295, #5357 ),
 .UNSPECIFIED., .F., .F. ) 
 B_SPLINE_CURVE_WITH_KNOTS ( ( 3, 2, 2, 2, 2, 3 ),
 ( 0.9333333333333333481, 0.9399999999999999467, 0.9466666666666666563, 0.9533333333333333659, 0.9599999999999999645, 0.9666666666666666741 ),
 .UNSPECIFIED. ) 
 CURVE ( )  GEOMETRIC_REPRESENTATION_ITEM ( )  RATIONAL_B_SPLINE_CURVE ( ( 1.000000000000000000, 0.9510565162951535312, 1.000000000000000000, 0.9510565162951535312, 1.000000000000000000, 0.9510565162951535312, 1.000000000000000000, 0.9510565162951535312, 1.000000000000000000, 0.9510565162951535312, 1.000000000000000000 ) ) 
 REPRESENTATION_ITEM ( '' )  );
#3786 = VECTOR ( 'NONE', #1135, 1000.000000000000000 ) ;
#3787 = CARTESIAN_POINT ( 'NONE',  ( 21.77500000054622831, 20.00000000000000355, 98.07665518445361386 ) ) ;
#3788 = DIRECTION ( 'NONE',  ( -1.000000000000000000, -0.000000000000000000, -0.000000000000000000 ) ) ;
#3789 = EDGE_CURVE ( 'NONE', #2899, #5337, #2990, .T. ) ;
#3790 = CARTESIAN_POINT ( 'NONE',  ( -4.999999999999999112, 50.32753737931852100, -20.39607805437113797 ) ) ;
#3791 = DIRECTION ( 'NONE',  ( 0.000000000000000000, -1.000000000000000000, 1.039664082171044875E-15 ) ) ;
#3792 = CARTESIAN_POINT ( 'NONE',  ( 2.217624749121678729, 45.50677551093724560, 27.91368483350839824 ) ) ;
#3793 = LINE ( 'NONE', #7670, #1041 ) ;
#3794 = ORIENTED_EDGE ( 'NONE', *, *, #5487, .T. ) ;
#3795 = CARTESIAN_POINT ( 'NONE',  ( 2.294321452706637121, 29.73876067080973229, -24.89658462890612967 ) ) ;
#3796 = AXIS2_PLACEMENT_3D ( 'NONE', #3687, #3628, #7567 ) ;
#3797 = APPLICATION_PROTOCOL_DEFINITION ( 'draft international standard', 'automotive_design', 1998, #11049 ) ;
#3798 = DIRECTION ( 'NONE',  ( 1.000000000000000000, 0.000000000000000000, 0.000000000000000000 ) ) ;
#3799 = CARTESIAN_POINT ( 'NONE',  ( 41.67500000054622689, 22.36655054427230027, 98.07665518445361386 ) ) ;
#3800 =( BOUNDED_CURVE ( )  B_SPLINE_CURVE ( 3, ( #4565, #4502, #3671, #5529 ),
 .UNSPECIFIED., .F., .F. ) 
 B_SPLINE_CURVE_WITH_KNOTS ( ( 4, 4 ),
 ( 0.2699327958334041266, 1.570796326794896558 ),
 .UNSPECIFIED. ) 
 CURVE ( )  GEOMETRIC_REPRESENTATION_ITEM ( )  RATIONAL_B_SPLINE_CURVE ( ( 1.000000000000000000, 0.8638816171694810864, 0.8638816171694810864, 1.000000000000000000 ) ) 
 REPRESENTATION_ITEM ( '' )  );
#3801 = AXIS2_PLACEMENT_3D ( 'NONE', #3486, #12431, #11475 ) ;
#3802 = CARTESIAN_POINT ( 'NONE',  ( 29.27500000054622475, 26.92701409722686634, 88.54243821818162985 ) ) ;
#3803 = CARTESIAN_POINT ( 'NONE',  ( 29.99999999999998934, 20.00000000000000355, 98.29316153445363113 ) ) ;
#3804 = EDGE_CURVE ( 'NONE', #1585, #4846, #4835, .T. ) ;
#3805 = CARTESIAN_POINT ( 'NONE',  ( 31.87500000054622973, 17.63344945572769973, 98.07665518445361386 ) ) ;
#3806 = EDGE_LOOP ( 'NONE', ( #3808, #2819 ) ) ;
#3807 = CARTESIAN_POINT ( 'NONE',  ( -50.00000000000001421, 22.00000000000000000, 188.4007504869563263 ) ) ;
#3808 = ORIENTED_EDGE ( 'NONE', *, *, #1641, .F. ) ;
#3809 = CARTESIAN_POINT ( 'NONE',  ( 6.843587254644259765, 12.70147400874256505, 19.85506230137591999 ) ) ;
#3810 = ORIENTED_EDGE ( 'NONE', *, *, #7903, .T. ) ;
#3811 = EDGE_CURVE ( 'NONE', #3410, #7937, #11162, .T. ) ;
#3812 = CARTESIAN_POINT ( 'NONE',  ( 42.25000000109246656, 12.86707612778636012, 88.47553407664152303 ) ) ;
#3813 = EDGE_CURVE ( 'NONE', #9971, #9039, #10972, .T. ) ;
#3814 = AXIS2_PLACEMENT_3D ( 'NONE', #2107, #1104, #5984 ) ;
#3815 = CARTESIAN_POINT ( 'NONE',  ( -2.000000000000015543, 20.00000000000000355, 90.79316153445363113 ) ) ;
#3816 = CARTESIAN_POINT ( 'NONE',  ( 2.615458182459051706, 10.32545218288117717, -27.88515796981556960 ) ) ;
#3817 = CARTESIAN_POINT ( 'NONE',  ( 44.97500000054621694, 22.36655054427230382, 83.50966788445364841 ) ) ;
#3818 = LINE ( 'NONE', #780, #12236 ) ;
#3819 = CARTESIAN_POINT ( 'NONE',  ( 32.00000000000000000, 0.000000000000000000, 5.035999999999999588 ) ) ;
#3820 = CARTESIAN_POINT ( 'NONE',  ( 44.17500000054622689, 13.80429023900056507, 95.29460816699764791 ) ) ;
#3821 = CARTESIAN_POINT ( 'NONE',  ( 21.07500000054622191, 24.28113015263587471, 84.90069139318163138 ) ) ;
#3822 = CARTESIAN_POINT ( 'NONE',  ( 39.69999999999998863, 26.37988106264029398, 95.42841645007781892 ) ) ;
#3823 = DIRECTION ( 'NONE',  ( -0.000000000000000000, 0.8660254037844395958, 0.4999999999999983902 ) ) ;
#3824 = AXIS2_PLACEMENT_3D ( 'NONE', #9746, #10883, #7840 ) ;
#3825 = ORIENTED_EDGE ( 'NONE', *, *, #5822, .F. ) ;
#3826 = CARTESIAN_POINT ( 'NONE',  ( 36.15000000109245804, 12.11403331821300533, 90.79316153445363113 ) ) ;
#3827 = CARTESIAN_POINT ( 'NONE',  ( 0.6578411763953998515, 54.96743791211429908, -24.99342793576595767 ) ) ;
#3828 = ORIENTED_EDGE ( 'NONE', *, *, #6489, .F. ) ;
#3829 = VECTOR ( 'NONE', #668, 1000.000000000000000 ) ;
#3830 = ORIENTED_EDGE ( 'NONE', *, *, #598, .F. ) ;
#3831 = EDGE_CURVE ( 'NONE', #9392, #11695, #11684, .T. ) ;
#3832 = CARTESIAN_POINT ( 'NONE',  ( -3.554546826686217020, 29.35267307038308360, -24.74790415999775917 ) ) ;
#3833 = CARTESIAN_POINT ( 'NONE',  ( 31.25000000109246656, 27.13292387221364876, 93.11078899226573924 ) ) ;
#3834 = CIRCLE ( 'NONE', #9319, 7.500000000000007105 ) ;
#3835 = CARTESIAN_POINT ( 'NONE',  ( 26.65000000109246514, 20.00000000000000355, 83.29316153445364534 ) ) ;
#3836 = VECTOR ( 'NONE', #12325, 1000.000000000000000 ) ;
#3837 = CARTESIAN_POINT ( 'NONE',  ( 35.07500000054623257, 26.19570976099943493, 86.29171490190961435 ) ) ;
#3838 = DIRECTION ( 'NONE',  ( 1.000000000000000000, 0.000000000000000000, 0.000000000000000000 ) ) ;
#3839 = CARTESIAN_POINT ( 'NONE',  ( -50.00000000000001421, 0.000000000000000000, 69.99999999999998579 ) ) ;
#3840 = VERTEX_POINT ( 'NONE', #1903 ) ;
#3841 = CARTESIAN_POINT ( 'NONE',  ( 4.839828837987002252, 51.29788161226999677, -27.57862052135422459 ) ) ;
#3842 = CARTESIAN_POINT ( 'NONE',  ( 48.35000000109246088, 13.62011893735970958, 86.15790661882942914 ) ) ;
#3843 = CARTESIAN_POINT ( 'NONE',  ( 48.27500000054622831, 13.07298590277314254, 93.04388485072563242 ) ) ;
#3844 = VERTEX_POINT ( 'NONE', #2095 ) ;
#3845 = FACE_OUTER_BOUND ( 'NONE', #4564, .T. ) ;
#3846 = CARTESIAN_POINT ( 'NONE',  ( 23.39999999999998792, 27.13292387221364876, 88.47553407664153724 ) ) ;
#3847 = VERTEX_POINT ( 'NONE', #11876 ) ;
#3848 = EDGE_LOOP ( 'NONE', ( #8448, #5912, #3182 ) ) ;
#3849 = LINE ( 'NONE', #7789, #5403 ) ;
#3850 = VECTOR ( 'NONE', #9098, 1000.000000000000114 ) ;
#3851 = DIRECTION ( 'NONE',  ( -1.000000000000000000, 0.000000000000000000, 0.000000000000000000 ) ) ;
#3852 = DIRECTION ( 'NONE',  ( -1.000000000000000000, -0.000000000000000000, -0.000000000000000000 ) ) ;
#3853 = EDGE_CURVE ( 'NONE', #10915, #10888, #3183, .T. ) ;
#3854 = CARTESIAN_POINT ( 'NONE',  ( 0.000000000000000000, 0.000000000000000000, -70.00000000000000000 ) ) ;
#3855 = CARTESIAN_POINT ( 'NONE',  ( -4.871666279273695999, 51.13754189277828743, -20.42713785987348984 ) ) ;
#3856 = CARTESIAN_POINT ( 'NONE',  ( 6.000000000000000000, 2.919948986426526005, -5.057500000000003659 ) ) ;
#3857 = CARTESIAN_POINT ( 'NONE',  ( 9.918037823481203219, 21.32003297329905678, -18.51037319129331848 ) ) ;
#3858 = CARTESIAN_POINT ( 'NONE',  ( 7.297088297540795132, 13.15481214220262274, 23.91253034306283354 ) ) ;
#3859 = VERTEX_POINT ( 'NONE', #10592 ) ;
#3860 = AXIS2_PLACEMENT_3D ( 'NONE', #4939, #187, #881 ) ;
#3861 = CARTESIAN_POINT ( 'NONE',  ( -0.3281837927571703561, 10.00000000000000711, -28.00000000000001066 ) ) ;
#3862 = UNCERTAINTY_MEASURE_WITH_UNIT (LENGTH_MEASURE( 1.000000000000000082E-05 ), #7814, 'distance_accuracy_value', 'NONE');
#3863 = CARTESIAN_POINT ( 'NONE',  ( 28.77500000054622831, 17.63344945572770328, 83.50966788445364841 ) ) ;
#3864 = DIRECTION ( 'NONE',  ( 0.000000000000000000, 0.000000000000000000, 1.000000000000000000 ) ) ;
#3865 = CARTESIAN_POINT ( 'NONE',  ( 40.27500000054622831, 12.34168156654572357, 90.79316153445363113 ) ) ;
#3866 = CARTESIAN_POINT ( 'NONE',  ( 24.57500000054622191, 13.80429023900056684, 86.29171490190961435 ) ) ;
#3867 = CARTESIAN_POINT ( 'NONE',  ( 25.19999999999998508, 24.40838939219355197, 84.72553407664153724 ) ) ;
#3868 = CONICAL_SURFACE ( 'NONE', #4680, 28.00000000000000000, 0.7853981633974477239 ) ;
#3869 = CARTESIAN_POINT ( 'NONE',  ( 34.17500000054622689, 13.07298590277314254, 93.04388485072563242 ) ) ;
#3870 = ORIENTED_EDGE ( 'NONE', *, *, #11183, .T. ) ;
#3871 = EDGE_CURVE ( 'NONE', #12073, #10081, #10747, .T. ) ;
#3872 = DIRECTION ( 'NONE',  ( 0.000000000000000000, 0.000000000000000000, -1.000000000000000000 ) ) ;
#3873 = EDGE_LOOP ( 'NONE', ( #1093, #95, #6888, #10917, #12199, #1219, #3957, #4192, #176, #9922, #27, #7249, #1890, #3065, #8872, #4330, #11997, #8265, #6433, #11806, #2633, #8670, #7385, #2230, #8226, #2860, #12409, #2942, #3054, #12415, #172, #3706, #327 ) ) ;
#3874 = CARTESIAN_POINT ( 'NONE',  ( 0.000000000000000000, 2.919948986426526005, -5.057500000000003659 ) ) ;
#3875 = ORIENTED_EDGE ( 'NONE', *, *, #3200, .T. ) ;
#3876 = SHAPE_REPRESENTATION_RELATIONSHIP ( 'NONE' , 'NONE' ,  #1739, #11260 ) ;
#3877 = DIRECTION ( 'NONE',  ( 1.000000000000000000, -0.000000000000000000, -0.000000000000000000 ) ) ;
#3878 = LINE ( 'NONE', #9785, #1749 ) ;
#3879 = CARTESIAN_POINT ( 'NONE',  ( 43.57500000054623257, 26.19570976099943849, 95.29460816699764791 ) ) ;
#3880 = LINE ( 'NONE', #10662, #1482 ) ;
#3881 = CARTESIAN_POINT ( 'NONE',  ( -50.00000000000001421, 0.000000000000000000, 69.99999999999998579 ) ) ;
#3882 = CARTESIAN_POINT ( 'NONE',  ( 46.97500000054621694, 22.36655054427230382, 83.50966788445364841 ) ) ;
#3883 = CARTESIAN_POINT ( 'NONE',  ( 48.19999999999998863, 15.59161060780645691, 96.86078899226572503 ) ) ;
#3884 = CARTESIAN_POINT ( 'NONE',  ( 45.59999999999998721, 27.13292387221364876, 93.11078899226573924 ) ) ;
#3885 = DIRECTION ( 'NONE',  ( 0.000000000000000000, 1.000000000000000000, 0.000000000000000000 ) ) ;
#3886 = ORIENTED_EDGE ( 'NONE', *, *, #8320, .F. ) ;
#3887 = EDGE_CURVE ( 'NONE', #574, #7418, #11746, .T. ) ;
#3888 = CARTESIAN_POINT ( 'NONE',  ( 30.95000000109246585, 26.37988106264029398, 86.15790661882942914 ) ) ;
#3889 = CARTESIAN_POINT ( 'NONE',  ( 0.000000000000000000, 1.065442715258197248E-15, -8.400000000000000355 ) ) ;
#3890 = EDGE_LOOP ( 'NONE', ( #12214, #4515, #12121, #8375, #4256 ) ) ;
#3891 = EDGE_CURVE ( 'NONE', #8158, #589, #7549, .T. ) ;
#3892 = ORIENTED_EDGE ( 'NONE', *, *, #5126, .F. ) ;
#3893 = FACE_OUTER_BOUND ( 'NONE', #8081, .T. ) ;
#3894 = EDGE_CURVE ( 'NONE', #3772, #513, #10150, .T. ) ;
#3895 = CARTESIAN_POINT ( 'NONE',  ( 0.000000000000000000, 20.00000000000000355, -28.00000000000000711 ) ) ;
#3896 = CARTESIAN_POINT ( 'NONE',  ( 38.97500000054622404, 24.28113015263587471, 84.90069139318163138 ) ) ;
#3897 = CARTESIAN_POINT ( 'NONE',  ( 38.37500000054622973, 12.34168156654572535, 90.79316153445363113 ) ) ;
#3898 = CARTESIAN_POINT ( 'NONE',  ( 35.05000000109246372, 27.13292387221364876, 88.47553407664153724 ) ) ;
#3899 = CARTESIAN_POINT ( 'NONE',  ( 6.608094568897072030, 27.51261231993640166, -27.21028944860474397 ) ) ;
#3900 = CARTESIAN_POINT ( 'NONE',  ( 6.000000000000000000, 0.000000000000000000, 0.000000000000000000 ) ) ;
#3901 = ORIENTED_EDGE ( 'NONE', *, *, #3563, .F. ) ;
#3902 = CARTESIAN_POINT ( 'NONE',  ( 49.55000000109246372, 22.43689772174679575, 98.29316153445363113 ) ) ;
#3903 = FACE_OUTER_BOUND ( 'NONE', #3806, .T. ) ;
#3904 = EDGE_LOOP ( 'NONE', ( #9429, #6032, #7106, #10703, #7655 ) ) ;
#3905 = DIRECTION ( 'NONE',  ( 0.000000000000000000, 0.000000000000000000, -1.000000000000000000 ) ) ;
#3906 = UNCERTAINTY_MEASURE_WITH_UNIT (LENGTH_MEASURE( 1.000000000000000082E-05 ), #10776, 'distance_accuracy_value', 'NONE');
#3907 = CARTESIAN_POINT ( 'NONE',  ( 6.000000000000000000, 0.000000000000000000, 0.000000000000000000 ) ) ;
#3908 = EDGE_LOOP ( 'NONE', ( #4928, #5155, #6598, #5137, #3177, #8373 ) ) ;
#3909 = APPLICATION_CONTEXT ( 'automotive_design' ) ;
#3910 = ORIENTED_EDGE ( 'NONE', *, *, #3894, .T. ) ;
#3911 = CARTESIAN_POINT ( 'NONE',  ( 42.95000000109246940, 26.37988106264029398, 86.15790661882942914 ) ) ;
#3912 = ADVANCED_FACE ( 'NONE', ( #5276 ), #9149, .T. ) ;
#3913 = CARTESIAN_POINT ( 'NONE',  ( -31.89339828220176898, 12.50000000000000711, 140.6066017177981848 ) ) ;
#3914 = LINE ( 'NONE', #8737, #8013 ) ;
#3915 = CARTESIAN_POINT ( 'NONE',  ( -10.00000000000000355, 20.00000000000000355, -26.15339366124404563 ) ) ;
#3916 = AXIS2_PLACEMENT_3D ( 'NONE', #2336, #12225, #4363 ) ;
#3917 = PLANE ( 'NONE',  #1318 ) ;
#3918 = CARTESIAN_POINT ( 'NONE',  ( -0.6578846949584694626, 54.95924935667866862, 20.99032885061396314 ) ) ;
#3919 = CARTESIAN_POINT ( 'NONE',  ( 5.000000000000000000, 50.00000000000000000, 27.54995462791182703 ) ) ;
#3920 = FACE_OUTER_BOUND ( 'NONE', #5666, .T. ) ;
#3921 = ORIENTED_EDGE ( 'NONE', *, *, #7766, .F. ) ;
#3922 = CARTESIAN_POINT ( 'NONE',  ( 36.95000000109246230, 26.37988106264029398, 86.15790661882942914 ) ) ;
#3923 = ADVANCED_FACE ( 'NONE', ( #6163 ), #1446, .F. ) ;
#3924 = CONTEXT_DEPENDENT_SHAPE_REPRESENTATION ( #6738, #4170 ) ;
#3925 = VECTOR ( 'NONE', #3960, 1000.000000000000000 ) ;
#3926 = VECTOR ( 'NONE', #7666, 1000.000000000000000 ) ;
#3927 = CARTESIAN_POINT ( 'NONE',  ( 21.37500000054622262, 27.65831843345427998, 90.79316153445363113 ) ) ;
#3928 = CARTESIAN_POINT ( 'NONE',  ( 49.57500000054621836, 26.19570976099943493, 95.29460816699764791 ) ) ;
#3929 = CARTESIAN_POINT ( 'NONE',  ( 40.17500000054623399, 13.07298590277314254, 93.04388485072563242 ) ) ;
#3930 = CARTESIAN_POINT ( 'NONE',  ( 19.87500000054622262, 20.00000000000000355, 98.07665518445361386 ) ) ;
#3931 = CARTESIAN_POINT ( 'NONE',  ( 25.09999999999998366, 22.43689772174679575, 83.29316153445363113 ) ) ;
#3932 = CARTESIAN_POINT ( 'NONE',  ( 27.49999999999999645, 20.00000000000000355, 187.9999999999999716 ) ) ;
#3933 = CARTESIAN_POINT ( 'NONE',  ( 36.17500000054622689, 13.07298590277314254, 93.04388485072563242 ) ) ;
#3934 = ORIENTED_EDGE ( 'NONE', *, *, #2384, .F. ) ;
#3935 = DIRECTION ( 'NONE',  ( 1.000000000000000000, 0.000000000000000000, 0.000000000000000000 ) ) ;
#3936 = ORIENTED_EDGE ( 'NONE', *, *, #939, .F. ) ;
#3937 = VECTOR ( 'NONE', #594, 1000.000000000000114 ) ;
#3938 = CARTESIAN_POINT ( 'NONE',  ( 0.3269428999352006482, 55.00000000000000711, 28.00000000000000711 ) ) ;
#3939 = VERTEX_POINT ( 'NONE', #3243 ) ;
#3940 = SHAPE_REPRESENTATION_RELATIONSHIP ( 'NONE' , 'NONE' ,  #10013, #4901 ) ;
#3941 = CARTESIAN_POINT ( 'NONE',  ( 10.40000000000000036, 0.000000000000000000, 5.000000000000000888 ) ) ;
#3942 = DIRECTION ( 'NONE',  ( -1.000000000000000000, -0.000000000000000000, -0.000000000000000000 ) ) ;
#3943 = CARTESIAN_POINT ( 'NONE',  ( 45.47500000054622404, 26.92701409722686634, 93.04388485072563242 ) ) ;
#3944 = CARTESIAN_POINT ( 'NONE',  ( 40.15000000109245804, 12.11403331821300533, 90.79316153445363113 ) ) ;
#3945 = EDGE_CURVE ( 'NONE', #4660, #2566, #2471, .T. ) ;
#3946 = DIRECTION ( 'NONE',  ( -0.7071067811865331398, 0.000000000000000000, 0.7071067811865617836 ) ) ;
#3947 = CARTESIAN_POINT ( 'NONE',  ( 44.89999999999998437, 17.56310227825321135, 83.29316153445363113 ) ) ;
#3948 = AXIS2_PLACEMENT_3D ( 'NONE', #5691, #1867, #858 ) ;
#3949 = CARTESIAN_POINT ( 'NONE',  ( 40.89999999999998437, 17.56310227825320425, 83.29316153445363113 ) ) ;
#3950 = FACE_OUTER_BOUND ( 'NONE', #9660, .T. ) ;
#3951 = EDGE_LOOP ( 'NONE', ( #12246, #10404, #11804, #11681 ) ) ;
#3952 = PRODUCT_RELATED_PRODUCT_CATEGORY ( 'part', '', ( #5783 ) ) ;
#3953 = ADVANCED_FACE ( 'NONE', ( #1525 ), #10213, .F. ) ;
#3954 = CARTESIAN_POINT ( 'NONE',  ( 32.75000000109245946, 22.43689772174679575, 83.29316153445363113 ) ) ;
#3955 = CARTESIAN_POINT ( 'NONE',  ( -2.618974170005213153, 10.32668121623932400, 24.87084347637328108 ) ) ;
#3956 = ORIENTED_EDGE ( 'NONE', *, *, #1801, .T. ) ;
#3957 = ORIENTED_EDGE ( 'NONE', *, *, #3417, .F. ) ;
#3958 = DIRECTION ( 'NONE',  ( 0.000000000000000000, 0.000000000000000000, -1.000000000000000000 ) ) ;
#3959 = CYLINDRICAL_SURFACE ( 'NONE', #1967, 10.00000000000000355 ) ;
#3960 = DIRECTION ( 'NONE',  ( 1.000000000000000000, 0.000000000000000000, 0.000000000000000000 ) ) ;
#3961 = CARTESIAN_POINT ( 'NONE',  ( 39.97500000054622404, 15.71886984736413417, 96.68563167572563088 ) ) ;
#3962 = CARTESIAN_POINT ( 'NONE',  ( 34.47500000054622404, 13.07298590277314432, 88.54243821818161564 ) ) ;
#3963 = CARTESIAN_POINT ( 'NONE',  ( -4.336936024885986285, 52.50935177099758278, 27.66269046005032095 ) ) ;
#3964 = CARTESIAN_POINT ( 'NONE',  ( -8.955040573717580443, 24.46236383193878083, 18.99568595680172578 ) ) ;
#3965 = CARTESIAN_POINT ( 'NONE',  ( 34.65000000109246514, 20.00000000000000355, 83.29316153445364534 ) ) ;
#3966 = VERTEX_POINT ( 'NONE', #6223 ) ;
#3967 = EDGE_CURVE ( 'NONE', #6721, #6252, #7108, .T. ) ;
#3968 = CARTESIAN_POINT ( 'NONE',  ( 4.743537283058001819, 51.61420199850529400, -24.54618281552716041 ) ) ;
#3969 = ORIENTED_EDGE ( 'NONE', *, *, #11568, .T. ) ;
#3970 = CARTESIAN_POINT ( 'NONE',  ( 34.99999999999998579, 20.00000000000000000, 137.5000000000000000 ) ) ;
#3971 = EDGE_LOOP ( 'NONE', ( #11474, #4080, #5367, #4409 ) ) ;
#3972 = ORIENTED_EDGE ( 'NONE', *, *, #958, .T. ) ;
#3973 = EDGE_CURVE ( 'NONE', #652, #11262, #3302, .T. ) ;
#3974 = CARTESIAN_POINT ( 'NONE',  ( 12.00000000000000178, 0.000000000000000000, 0.000000000000000000 ) ) ;
#3975 = LINE ( 'NONE', #1011, #9668 ) ;
#3976 = CARTESIAN_POINT ( 'NONE',  ( 9.685019593098569857, 22.50223202666526134, 97.86792408789433750 ) ) ;
#3977 = DIRECTION ( 'NONE',  ( 0.000000000000000000, 0.000000000000000000, 1.000000000000000000 ) ) ;
#3978 = FACE_OUTER_BOUND ( 'NONE', #6820, .T. ) ;
#3979 = FACE_OUTER_BOUND ( 'NONE', #6761, .T. ) ;
#3980 = AXIS2_PLACEMENT_3D ( 'NONE', #6274, #1692, #11277 ) ;
#3981 = CARTESIAN_POINT ( 'NONE',  ( -24.10660171779822747, 69.50000000000000000, 151.2467237978899846 ) ) ;
#3982 = CARTESIAN_POINT ( 'NONE',  ( 41.87500000054622262, 17.63344945572769973, 98.07665518445361386 ) ) ;
#3983 = DIRECTION ( 'NONE',  ( 1.000000000000000000, -0.000000000000000000, -0.000000000000000000 ) ) ;
#3984 = ORIENTED_EDGE ( 'NONE', *, *, #1388, .F. ) ;
#3985 = CARTESIAN_POINT ( 'NONE',  ( 36.75000000109246656, 22.43689772174676023, 83.29316153445360271 ) ) ;
#3986 = PRODUCT_CONTEXT ( 'NONE', #8218, 'mechanical' ) ;
#3987 = AXIS2_PLACEMENT_3D ( 'NONE', #10570, #748, #8488 ) ;
#3988 = CARTESIAN_POINT ( 'NONE',  ( 46.09999999999998010, 17.56310227825323977, 98.29316153445364534 ) ) ;
#3989 = DIRECTION ( 'NONE',  ( 1.000000000000000000, 0.000000000000000000, 0.000000000000000000 ) ) ;
#3990 = CARTESIAN_POINT ( 'NONE',  ( 30.27500000054622831, 12.34168156654572357, 90.79316153445363113 ) ) ;
#3991 = CARTESIAN_POINT ( 'NONE',  ( 4.452539714567801177, 11.03997247681473404, -24.60205477162727661 ) ) ;
#3992 = CARTESIAN_POINT ( 'NONE',  ( 20.79999999999999005, 15.59161060780646046, 84.72553407664153724 ) ) ;
#3993 = DIRECTION ( 'NONE',  ( 1.000000000000000000, -0.000000000000000000, -0.000000000000000000 ) ) ;
#3994 = CARTESIAN_POINT ( 'NONE',  ( 30.67500000054622689, 17.63344945572770328, 83.50966788445364841 ) ) ;
#3995 = ORIENTED_EDGE ( 'NONE', *, *, #10753, .T. ) ;
#3996 = PLANE ( 'NONE',  #9125 ) ;
#3997 = CIRCLE ( 'NONE', #9481, 5.057500000000000107 ) ;
#3998 = ORIENTED_EDGE ( 'NONE', *, *, #11974, .T. ) ;
#3999 = CARTESIAN_POINT ( 'NONE',  ( 3.303823242547402117, 53.76705800516405276, 27.80537070972012259 ) ) ;
#4000 = ORIENTED_EDGE ( 'NONE', *, *, #3765, .F. ) ;
#4001 = CARTESIAN_POINT ( 'NONE',  ( -3.050747483057216769, 53.97487283205587261, -24.81466456749452831 ) ) ;
#4002 = CYLINDRICAL_SURFACE ( 'NONE', #11913, 7.499999999999992895 ) ;
#4003 = CARTESIAN_POINT ( 'NONE',  ( 35.87500000054622973, 20.00000000000000355, 98.07665518445361386 ) ) ;
#4004 = CARTESIAN_POINT ( 'NONE',  ( 121.9999999999999858, 0.000000000000000000, 0.000000000000000000 ) ) ;
#4005 = FACE_OUTER_BOUND ( 'NONE', #485, .T. ) ;
#4006 = CARTESIAN_POINT ( 'NONE',  ( 41.87500000054622262, 20.00000000000000355, 98.07665518445361386 ) ) ;
#4007 = CARTESIAN_POINT ( 'NONE',  ( 44.99999999999999289, 20.00000000000000355, 83.29316153445364534 ) ) ;
#4008 = CARTESIAN_POINT ( 'NONE',  ( -8.980220477185385519, 24.44733350940715866, -23.33298399582670157 ) ) ;
#4009 = EDGE_CURVE ( 'NONE', #3211, #7244, #7167, .T. ) ;
#4010 = FACE_OUTER_BOUND ( 'NONE', #1123, .T. ) ;
#4011 = VERTEX_POINT ( 'NONE', #9273 ) ;
#4012 = CARTESIAN_POINT ( 'NONE',  ( 33.45000000109246940, 24.40838939219354842, 96.86078899226572503 ) ) ;
#4013 = FACE_OUTER_BOUND ( 'NONE', #5018, .T. ) ;
#4014 = ORIENTED_EDGE ( 'NONE', *, *, #8243, .T. ) ;
#4015 = VECTOR ( 'NONE', #7321, 1000.000000000000114 ) ;
#4016 = ORIENTED_EDGE ( 'NONE', *, *, #9752, .T. ) ;
#4017 = MECHANICAL_DESIGN_GEOMETRIC_PRESENTATION_REPRESENTATION (  '', ( #9498 ), #1395 ) ;
#4018 = CARTESIAN_POINT ( 'NONE',  ( 4.442227524869980293, 11.03487569001018009, 27.64691637681915282 ) ) ;
#4019 = DIRECTION ( 'NONE',  ( 0.000000000000000000, 0.000000000000000000, -1.000000000000000000 ) ) ;
#4020 = DIRECTION ( 'NONE',  ( 0.000000000000000000, 0.000000000000000000, 1.000000000000000000 ) ) ;
#4021 = AXIS2_PLACEMENT_3D ( 'NONE', #9450, #5706, #7539 ) ;
#4022 = CARTESIAN_POINT ( 'NONE',  ( 30.17500000054623044, 13.07298590277314254, 93.04388485072563242 ) ) ;
#4023 = CARTESIAN_POINT ( 'NONE',  ( 34.57500000054621125, 13.80429023900056684, 86.29171490190961435 ) ) ;
#4024 = UNCERTAINTY_MEASURE_WITH_UNIT (LENGTH_MEASURE( 1.000000000000000082E-05 ), #12066, 'distance_accuracy_value', 'NONE');
#4025 = CIRCLE ( 'NONE', #7680, 10.00000000000000888 ) ;
#4026 = CARTESIAN_POINT ( 'NONE',  ( 3.236409131694046426, 29.46755692282902928, -27.81414090612697976 ) ) ;
#4027 = DIRECTION ( 'NONE',  ( 0.000000000000000000, 0.000000000000000000, -1.000000000000000000 ) ) ;
#4028 = ORIENTED_EDGE ( 'NONE', *, *, #2398, .F. ) ;
#4029 = CARTESIAN_POINT ( 'NONE',  ( 47.45000000109246230, 24.40838939219354842, 96.86078899226572503 ) ) ;
#4030 = DIRECTION ( 'NONE',  ( 0.000000000000000000, 0.000000000000000000, 1.000000000000000000 ) ) ;
#4031 = ORIENTED_EDGE ( 'NONE', *, *, #1107, .T. ) ;
#4032 = DIRECTION ( 'NONE',  ( -1.224646799147353207E-16, 1.000000000000000000, 0.000000000000000000 ) ) ;
#4033 = EDGE_CURVE ( 'NONE', #8859, #8129, #826, .T. ) ;
#4034 = ORIENTED_EDGE ( 'NONE', *, *, #8993, .T. ) ;
#4035 = AXIS2_PLACEMENT_3D ( 'NONE', #1743, #5624, #800 ) ;
#4036 = DIRECTION ( 'NONE',  ( -1.000000000000000000, 0.000000000000000000, -0.000000000000000000 ) ) ;
#4037 = CARTESIAN_POINT ( 'NONE',  ( 36.99999999999995026, 0.000000000000000000, 69.99999999999998579 ) ) ;
#4038 = EDGE_CURVE ( 'NONE', #1723, #1521, #12184, .T. ) ;
#4039 = CARTESIAN_POINT ( 'NONE',  ( 9.796548249817144338, 22.02198220144915553, 98.01984945353935075 ) ) ;
#4040 = CARTESIAN_POINT ( 'NONE',  ( -2.000000000000015543, 20.00000000000000355, 83.29316153445364534 ) ) ;
#4041 = CARTESIAN_POINT ( 'NONE',  ( -0.3266958997752330562, 45.00000000000001421, -25.00000000000000355 ) ) ;
#4042 = CARTESIAN_POINT ( 'NONE',  ( -3.973286137925955863, 53.05282384735495782, 20.62152687101385951 ) ) ;
#4043 = EDGE_CURVE ( 'NONE', #3859, #2987, #29, .T. ) ;
#4044 = LINE ( 'NONE', #9955, #1928 ) ;
#4045 = CARTESIAN_POINT ( 'NONE',  ( 40.57500000054623257, 15.71886984736413773, 84.90069139318163138 ) ) ;
#4046 = LINE ( 'NONE', #9765, #10538 ) ;
#4047 = ORIENTED_EDGE ( 'NONE', *, *, #3361, .T. ) ;
#4048 = CARTESIAN_POINT ( 'NONE',  ( 5.034037828167091000, 28.66467738801596354, -24.49412005228846922 ) ) ;
#4049 = EDGE_CURVE ( 'NONE', #4582, #5275, #4890, .T. ) ;
#4050 = CARTESIAN_POINT ( 'NONE',  ( 21.57500000054622191, 26.19570976099943849, 95.29460816699764791 ) ) ;
#4051 = DIRECTION ( 'NONE',  ( 1.000000000000000000, 0.000000000000000000, 0.000000000000000000 ) ) ;
#4052 = CARTESIAN_POINT ( 'NONE',  ( 36.27500000054622831, 12.34168156654572357, 90.79316153445363113 ) ) ;
#4053 = CARTESIAN_POINT ( 'NONE',  ( 21.67500000054622333, 24.28113015263587116, 96.68563167572563088 ) ) ;
#4054 = CARTESIAN_POINT ( 'NONE',  ( 23.89999999999998792, 22.43689772174679575, 98.29316153445363113 ) ) ;
#4055 = DIRECTION ( 'NONE',  ( 0.000000000000000000, 0.000000000000000000, -1.000000000000000000 ) ) ;
#4056 = CARTESIAN_POINT ( 'NONE',  ( 32.17500000054622689, 13.07298590277314254, 93.04388485072563242 ) ) ;
#4057 = VERTEX_POINT ( 'NONE', #7044 ) ;
#4058 = AXIS2_PLACEMENT_3D ( 'NONE', #11412, #2662, #1522 ) ;
#4059 = PRODUCT_DEFINITION_SHAPE ( 'NONE', 'NONE',  #7910 ) ;
#4060 = CARTESIAN_POINT ( 'NONE',  ( 0.000000000000000000, 20.00000000000000355, 106.9999999999999574 ) ) ;
#4061 = FACE_OUTER_BOUND ( 'NONE', #901, .T. ) ;
#4062 = EDGE_LOOP ( 'NONE', ( #11400, #5448 ) ) ;
#4063 = CARTESIAN_POINT ( 'NONE',  ( 0.000000000000000000, 20.00000000000000355, -66.99999999999998579 ) ) ;
#4064 = VERTEX_POINT ( 'NONE', #10159 ) ;
#4065 = DIRECTION ( 'NONE',  ( 0.000000000000000000, 0.4999999999999987232, -0.8660254037844392627 ) ) ;
#4066 = CARTESIAN_POINT ( 'NONE',  ( 9.674670850494081265, 17.38628865587025984, -26.27584064538169173 ) ) ;
#4067 = VECTOR ( 'NONE', #6791, 1000.000000000000000 ) ;
#4068 = CARTESIAN_POINT ( 'NONE',  ( 39.97500000054622404, 17.63344945572769973, 98.07665518445361386 ) ) ;
#4069 = CARTESIAN_POINT ( 'NONE',  ( -50.00000000000001421, 20.00000000000000000, 145.0000000000000000 ) ) ;
#4070 = LINE ( 'NONE', #399, #11662 ) ;
#4071 = CARTESIAN_POINT ( 'NONE',  ( 39.77500000054621410, 22.36655054427230027, 98.07665518445361386 ) ) ;
#4072 = CARTESIAN_POINT ( 'NONE',  ( 40.39999999999999147, 12.86707612778636012, 93.11078899226572503 ) ) ;
#4073 = CARTESIAN_POINT ( 'NONE',  ( 6.000000000000000000, 4.379923479639795225, -2.528750000000006271 ) ) ;
#4074 = CARTESIAN_POINT ( 'NONE',  ( -20.00000000000001776, 20.00000000000000000, 137.5000000000000000 ) ) ;
#4075 = ORIENTED_EDGE ( 'NONE', *, *, #67, .T. ) ;
#4076 = CARTESIAN_POINT ( 'NONE',  ( 32.65000000109246514, 20.00000000000000355, 83.29316153445364534 ) ) ;
#4077 = DIRECTION ( 'NONE',  ( 0.000000000000000000, 0.4999999999999983902, -0.8660254037844395958 ) ) ;
#4078 = ORIENTED_EDGE ( 'NONE', *, *, #6365, .T. ) ;
#4079 = EDGE_CURVE ( 'NONE', #5036, #11133, #8337, .T. ) ;
#4080 = ORIENTED_EDGE ( 'NONE', *, *, #5795, .T. ) ;
#4081 = ADVANCED_FACE ( 'NONE', ( #10919 ), #2236, .T. ) ;
#4082 = CARTESIAN_POINT ( 'NONE',  ( 25.45000000109246230, 24.40838939219354842, 96.86078899226572503 ) ) ;
#4083 = CARTESIAN_POINT ( 'NONE',  ( -3.973726775714538029, 53.05247132632594287, -24.68286527305685141 ) ) ;
#4084 = EDGE_CURVE ( 'NONE', #1716, #3396, #3800, .T. ) ;
#4085 = DIRECTION ( 'NONE',  ( 0.000000000000000000, -1.000000000000000000, -0.000000000000000000 ) ) ;
#4086 = CARTESIAN_POINT ( 'NONE',  ( 29.27500000054622831, 27.65831843345427998, 90.79316153445363113 ) ) ;
#4087 = CARTESIAN_POINT ( 'NONE',  ( 32.47500000054621694, 13.07298590277314432, 88.54243821818161564 ) ) ;
#4088 = LINE ( 'NONE', #5051, #7172 ) ;
#4089 = CARTESIAN_POINT ( 'NONE',  ( 9.935543424393982193, 21.31157940332991174, -26.17831177576534785 ) ) ;
#4090 = CARTESIAN_POINT ( 'NONE',  ( 34.25000000109245946, 12.86707612778636012, 88.47553407664152303 ) ) ;
#4091 = ORIENTED_EDGE ( 'NONE', *, *, #1755, .F. ) ;
#4092 = CARTESIAN_POINT ( 'NONE',  ( 48.27500000054622831, 13.07298590277314254, 93.04388485072563242 ) ) ;
#4093 = CARTESIAN_POINT ( 'NONE',  ( 48.45000000109246940, 15.59161060780646046, 84.72553407664153724 ) ) ;
#4094 = ORIENTED_EDGE ( 'NONE', *, *, #612, .F. ) ;
#4095 = CARTESIAN_POINT ( 'NONE',  ( 30.65000000109246514, 20.00000000000000355, 83.29316153445364534 ) ) ;
#4096 = ORIENTED_EDGE ( 'NONE', *, *, #7443, .F. ) ;
#4097 = DIRECTION ( 'NONE',  ( 0.000000000000000000, 0.7071067811865474617, 0.7071067811865474617 ) ) ;
#4098 = CARTESIAN_POINT ( 'NONE',  ( -10.00000000000000355, 20.00000000000000355, -18.46618531261938401 ) ) ;
#4099 = DIRECTION ( 'NONE',  ( 0.000000000000000000, 1.000000000000000000, -1.224646799147353207E-16 ) ) ;
#4100 = CARTESIAN_POINT ( 'NONE',  ( 0.3299754220453550713, 55.00000000000001421, 25.00000000000000000 ) ) ;
#4101 = ADVANCED_FACE ( 'NONE', ( #11415 ), #7524, .F. ) ;
#4102 = CARTESIAN_POINT ( 'NONE',  ( 7.415375966899784288, 26.71411643570026229, 94.16958235496709051 ) ) ;
#4103 = DIRECTION ( 'NONE',  ( 0.000000000000000000, 0.000000000000000000, -1.000000000000000000 ) ) ;
#4104 = CARTESIAN_POINT ( 'NONE',  ( -4.484481976314367735, 47.78274414339135490, -24.59462526944309246 ) ) ;
#4105 = DIRECTION ( 'NONE',  ( 1.000000000000000000, -0.000000000000000000, -0.000000000000000000 ) ) ;
#4106 = CARTESIAN_POINT ( 'NONE',  ( -2.220574438802248807, 45.50813311347688739, 27.91346354743601310 ) ) ;
#4107 = CARTESIAN_POINT ( 'NONE',  ( 44.57500000054622546, 15.71886984736413773, 84.90069139318163138 ) ) ;
#4108 = ADVANCED_FACE ( 'NONE', ( #6525 ), #4690, .F. ) ;
#4109 = AXIS2_PLACEMENT_3D ( 'NONE', #5343, #459, #12128 ) ;
#4110 = CARTESIAN_POINT ( 'NONE',  ( -2.509809017951089682, 45.66333224303983229, -24.87518608377025231 ) ) ;
#4111 = ORIENTED_EDGE ( 'NONE', *, *, #5665, .F. ) ;
#4112 = CARTESIAN_POINT ( 'NONE',  ( 0.000000000000000000, 4.685197434473814759, -5.637851296924623057E-15 ) ) ;
#4113 = ITEM_DEFINED_TRANSFORMATION ( 'NONE', 'NONE', #11831,  #9021 ) ;
#4114 = CARTESIAN_POINT ( 'NONE',  ( 22.67500000054622333, 15.71886984736413773, 84.90069139318163138 ) ) ;
#4115 = CARTESIAN_POINT ( 'NONE',  ( 49.07500000054622546, 24.28113015263587471, 84.90069139318163138 ) ) ;
#4116 = AXIS2_PLACEMENT_3D ( 'NONE', #7652, #11585, #12411 ) ;
#4117 = CARTESIAN_POINT ( 'NONE',  ( 34.97500000054623115, 24.28113015263587471, 84.90069139318163138 ) ) ;
#4118 = CARTESIAN_POINT ( 'NONE',  ( 21.97500000054622049, 17.63344945572769973, 98.07665518445361386 ) ) ;
#4119 = CARTESIAN_POINT ( 'NONE',  ( 21.39999999999998792, 27.13292387221364876, 88.47553407664153724 ) ) ;
#4120 = DIRECTION ( 'NONE',  ( 0.000000000000000000, -0.4999999999999990008, 0.8660254037844391517 ) ) ;
#4121 = CARTESIAN_POINT ( 'NONE',  ( 24.17500000054622689, 13.07298590277314254, 93.04388485072563242 ) ) ;
#4122 = ORIENTED_EDGE ( 'NONE', *, *, #1627, .T. ) ;
#4123 = EDGE_CURVE ( 'NONE', #6453, #1585, #1706, .T. ) ;
#4124 = CARTESIAN_POINT ( 'NONE',  ( 6.000000000000000000, -5.258101095580057891E-15, -5.057500000000000107 ) ) ;
#4125 = ORIENTED_EDGE ( 'NONE', *, *, #1303, .F. ) ;
#4126 = VERTEX_POINT ( 'NONE', #3729 ) ;
#4127 = DIRECTION ( 'NONE',  ( 0.000000000000000000, 0.000000000000000000, -1.000000000000000000 ) ) ;
#4128 = VERTEX_POINT ( 'NONE', #7421 ) ;
#4129 = AXIS2_PLACEMENT_3D ( 'NONE', #2052, #6057, #5932 ) ;
#4130 =( LENGTH_UNIT ( ) NAMED_UNIT ( * ) SI_UNIT ( .MILLI., .METRE. ) );
#4131 = CIRCLE ( 'NONE', #11219, 10.00000000000000355 ) ;
#4132 = CARTESIAN_POINT ( 'NONE',  ( -4.999999999999999112, 50.32713193883511593, -24.49489742783179125 ) ) ;
#4133 = CARTESIAN_POINT ( 'NONE',  ( 5.340684424226280325E-17, 55.00000000000000000, -25.00000000000000000 ) ) ;
#4134 = EDGE_CURVE ( 'NONE', #8484, #1332, #10394, .T. ) ;
#4135 = CARTESIAN_POINT ( 'NONE',  ( 40.67500000054622689, 15.71886984736413773, 84.90069139318163138 ) ) ;
#4136 = PLANE ( 'NONE',  #9184 ) ;
#4137 = CARTESIAN_POINT ( 'NONE',  ( -3.764971525938848540, 46.69375435830438192, -27.74669386146050698 ) ) ;
#4138 = CARTESIAN_POINT ( 'NONE',  ( 41.47500000054623115, 26.92701409722686634, 93.04388485072563242 ) ) ;
#4139 = CARTESIAN_POINT ( 'NONE',  ( 43.99999999999999289, 20.00000000000000355, 98.29316153445363113 ) ) ;
#4140 = CARTESIAN_POINT ( 'NONE',  ( 45.47500000054623825, 26.19570976099943493, 95.29460816699764791 ) ) ;
#4141 = ORIENTED_EDGE ( 'NONE', *, *, #3831, .F. ) ;
#4142 = AXIS2_PLACEMENT_3D ( 'NONE', #9560, #12533, #861 ) ;
#4143 = CARTESIAN_POINT ( 'NONE',  ( 25.85000000109246443, 15.59161060780645691, 96.86078899226572503 ) ) ;
#4144 = LINE ( 'NONE', #8837, #7908 ) ;
#4145 = VERTEX_POINT ( 'NONE', #2534 ) ;
#4146 =( BOUNDED_CURVE ( )  B_SPLINE_CURVE ( 2, ( #2734, #6719, #10714, #893, #9654, #961, #11612, #8751, #1963, #4891, #6593 ),
 .UNSPECIFIED., .F., .F. ) 
 B_SPLINE_CURVE_WITH_KNOTS ( ( 3, 2, 2, 2, 2, 3 ),
 ( 0.5000000000000000000, 0.5066666666666667096, 0.5133333333333333082, 0.5200000000000000178, 0.5266666666666666163, 0.5333333333333333259 ),
 .UNSPECIFIED. ) 
 CURVE ( )  GEOMETRIC_REPRESENTATION_ITEM ( )  RATIONAL_B_SPLINE_CURVE ( ( 1.000000000000000000, 0.9510565162951535312, 1.000000000000000000, 0.9510565162951535312, 1.000000000000000000, 0.9510565162951535312, 1.000000000000000000, 0.9510565162951535312, 1.000000000000000000, 0.9510565162951535312, 1.000000000000000000 ) ) 
 REPRESENTATION_ITEM ( '' )  );
#4147 = CARTESIAN_POINT ( 'NONE',  ( 2.222400765636041164, 54.49077458862202405, -20.88425590885463379 ) ) ;
#4148 = VERTEX_POINT ( 'NONE', #8436 ) ;
#4149 = CARTESIAN_POINT ( 'NONE',  ( 5.300979503027939188, 11.51433960415130997, 27.49502322044257241 ) ) ;
#4150 = CARTESIAN_POINT ( 'NONE',  ( -4.839726511208201742, 51.29827509403275343, -24.52715513826036897 ) ) ;
#4151 = CARTESIAN_POINT ( 'NONE',  ( -50.00000000000001421, 20.00000000000000000, 137.5000000000000000 ) ) ;
#4152 = AXIS2_PLACEMENT_3D ( 'NONE', #920, #7580, #5741 ) ;
#4153 = CARTESIAN_POINT ( 'NONE',  ( 28.47500000054622404, 13.80429023900056684, 86.29171490190961435 ) ) ;
#4154 = CARTESIAN_POINT ( 'NONE',  ( 28.67500000054622689, 15.71886984736413773, 84.90069139318163138 ) ) ;
#4155 = CARTESIAN_POINT ( 'NONE',  ( -4.967267959664427579, 50.65835542335811681, 27.55595201800184313 ) ) ;
#4156 = CARTESIAN_POINT ( 'NONE',  ( 3.061617454482527662E-15, 30.00000000000001066, 25.00000000000000000 ) ) ;
#4157 = CARTESIAN_POINT ( 'NONE',  ( -27.49999999999999645, 20.00000000000000355, 99.99999999999997158 ) ) ;
#4158 = EDGE_LOOP ( 'NONE', ( #11462, #1236, #8774, #9016 ) ) ;
#4159 = CARTESIAN_POINT ( 'NONE',  ( 47.55000000109247082, 22.43689772174679575, 98.29316153445363113 ) ) ;
#4160 = EDGE_LOOP ( 'NONE', ( #12079, #11105, #6997, #9283, #11649, #1574, #8132, #4437, #11447 ) ) ;
#4161 = EDGE_CURVE ( 'NONE', #11790, #9272, #9520, .T. ) ;
#4162 = CARTESIAN_POINT ( 'NONE',  ( 0.6000000000000033085, 0.000000000000000000, 0.000000000000000000 ) ) ;
#4163 = VECTOR ( 'NONE', #1012, 1000.000000000000000 ) ;
#4164 = EDGE_LOOP ( 'NONE', ( #1794, #4301 ) ) ;
#4165 = AXIS2_PLACEMENT_3D ( 'NONE', #3638, #6617, #9845 ) ;
#4166 = CARTESIAN_POINT ( 'NONE',  ( -9.983226034450831676, 19.33178880168245328, -18.47529793303663936 ) ) ;
#4167 = DIRECTION ( 'NONE',  ( 0.000000000000000000, 0.000000000000000000, -1.000000000000000000 ) ) ;
#4168 = VECTOR ( 'NONE', #4065, 1000.000000000000227 ) ;
#4169 = CYLINDRICAL_SURFACE ( 'NONE', #2980, 7.500000000000000000 ) ;
#4170 = PRODUCT_DEFINITION_SHAPE ( 'NONE', 'NONE',  #12542 ) ;
#4171 = CARTESIAN_POINT ( 'NONE',  ( 6.614416936062160524, 27.49996590649457673, 90.53406983787975548 ) ) ;
#4172 = CARTESIAN_POINT ( 'NONE',  ( -6.999999999999999112, 55.00000000000000000, 147.8533255156883399 ) ) ;
#4173 = LINE ( 'NONE', #11725, #4957 ) ;
#4174 = CARTESIAN_POINT ( 'NONE',  ( -50.00000000000001421, 22.00000000000000000, 152.2284161474004520 ) ) ;
#4175 = EDGE_CURVE ( 'NONE', #5701, #3634, #6587, .T. ) ;
#4176 = CARTESIAN_POINT ( 'NONE',  ( 1.342157722727130131E-15, 30.00000000000002132, -21.00000000000000355 ) ) ;
#4177 = CARTESIAN_POINT ( 'NONE',  ( 45.47500000054623825, 26.19570976099943493, 95.29460816699764791 ) ) ;
#4178 = CARTESIAN_POINT ( 'NONE',  ( 6.000000000000000000, 2.919948986426526005, -5.057500000000003659 ) ) ;
#4179 = ORIENTED_EDGE ( 'NONE', *, *, #7811, .T. ) ;
#4180 = CARTESIAN_POINT ( 'NONE',  ( -3.049660161009143611, 53.97562969122508747, 24.81478968795947537 ) ) ;
#4181 = ADVANCED_FACE ( 'NONE', ( #10271 ), #819, .T. ) ;
#4182 = CARTESIAN_POINT ( 'NONE',  ( 23.57500000054622191, 26.19570976099943849, 95.29460816699764791 ) ) ;
#4183 = CARTESIAN_POINT ( 'NONE',  ( 42.37500000054621552, 12.34168156654572535, 90.79316153445363113 ) ) ;
#4184 = VECTOR ( 'NONE', #4491, 1000.000000000000000 ) ;
#4185 = CARTESIAN_POINT ( 'NONE',  ( 31.87500000054622973, 17.63344945572769973, 98.07665518445361386 ) ) ;
#4186 = CARTESIAN_POINT ( 'NONE',  ( 19.97500000054622404, 17.63344945572769973, 98.07665518445361386 ) ) ;
#4187 = LINE ( 'NONE', #6339, #11532 ) ;
#4188 =( NAMED_UNIT ( * ) PLANE_ANGLE_UNIT ( ) SI_UNIT ( $, .RADIAN. ) );
#4189 = CARTESIAN_POINT ( 'NONE',  ( 24.57500000054622902, 15.71886984736413773, 84.90069139318163138 ) ) ;
#4190 = ORIENTED_EDGE ( 'NONE', *, *, #5188, .F. ) ;
#4191 = DIRECTION ( 'NONE',  ( 1.000000000000000000, 0.000000000000000000, 0.000000000000000000 ) ) ;
#4192 = ORIENTED_EDGE ( 'NONE', *, *, #2114, .F. ) ;
#4193 = EDGE_LOOP ( 'NONE', ( #3096, #6299 ) ) ;
#4194 = CARTESIAN_POINT ( 'NONE',  ( 38.59999999999998721, 12.86707612778636012, 88.47553407664152303 ) ) ;
#4195 = ORIENTED_EDGE ( 'NONE', *, *, #12508, .F. ) ;
#4196 = EDGE_CURVE ( 'NONE', #6070, #5277, #8620, .T. ) ;
#4197 = AXIS2_PLACEMENT_3D ( 'NONE', #1945, #11661, #3087 ) ;
#4198 = B_SPLINE_CURVE_WITH_KNOTS ( 'NONE', 3,
 ( #2078, #4819, #5008, #11671, #1144, #9705, #5898, #2147, #4941, #2849, #9896, #11733, #9643, #1020, #8745, #6776, #10642, #4048, #8807, #10834, #5773, #7926, #3795, #4881, #950, #11602, #8685, #3036 ),
 .UNSPECIFIED., .F., .F.,
 ( 4, 2, 2, 2, 2, 2, 2, 2, 2, 2, 2, 2, 2, 4 ),
 ( 0.04738924854463780201, 0.04936272659091893444, 0.05034946561405949372, 0.05133620463720005994, 0.05232294366034062616, 0.05330968268348119238, 0.05528316072976231788, 0.05626989975290288409, 0.05725663877604345031, 0.05923011682232458969, 0.06021685584546515591, 0.06120359486860571518, 0.06219033389174628140, 0.06317707291488684762 ),
 .UNSPECIFIED. ) ;
#4199 = CARTESIAN_POINT ( 'NONE',  ( 0.000000000000000000, 0.000000000000000000, 69.99999999999998579 ) ) ;
#4200 = CARTESIAN_POINT ( 'NONE',  ( 39.87500000054622262, 20.00000000000000355, 98.07665518445361386 ) ) ;
#4201 = CARTESIAN_POINT ( 'NONE',  ( -0.3308735998258449107, 55.00000000000001421, -28.00000000000001066 ) ) ;
#4202 = ADVANCED_FACE ( 'NONE', ( #5586 ), #10493, .T. ) ;
#4203 = CARTESIAN_POINT ( 'NONE',  ( 26.39999999999998792, 12.86707612778636012, 93.11078899226572503 ) ) ;
#4204 = CARTESIAN_POINT ( 'NONE',  ( 37.97500000054621694, 17.63344945572769973, 98.07665518445361386 ) ) ;
#4205 = CARTESIAN_POINT ( 'NONE',  ( 40.59999999999998721, 12.86707612778636012, 88.47553407664152303 ) ) ;
#4206 = VECTOR ( 'NONE', #7834, 1000.000000000000000 ) ;
#4207 = CARTESIAN_POINT ( 'NONE',  ( 47.87500000054622973, 17.63344945572769973, 98.07665518445361386 ) ) ;
#4208 = ORIENTED_EDGE ( 'NONE', *, *, #12157, .F. ) ;
#4209 = CARTESIAN_POINT ( 'NONE',  ( 26.15000000109246159, 12.11403331821300533, 90.79316153445363113 ) ) ;
#4210 = CARTESIAN_POINT ( 'NONE',  ( 5.000000000000000000, 0.000000000000000000, 0.000000000000000000 ) ) ;
#4211 = ORIENTED_EDGE ( 'NONE', *, *, #2572, .F. ) ;
#4212 = EDGE_CURVE ( 'NONE', #12368, #6993, #8674, .T. ) ;
#4213 = EDGE_CURVE ( 'NONE', #10247, #6828, #12371, .T. ) ;
#4214 = CARTESIAN_POINT ( 'NONE',  ( -9.741195869257412099, 22.28434334298316699, -26.25097870757294416 ) ) ;
#4215 = ORIENTED_EDGE ( 'NONE', *, *, #5834, .T. ) ;
#4216 = CARTESIAN_POINT ( 'NONE',  ( 2.284872756015303707, 10.25892335484974538, 27.90850932234814152 ) ) ;
#4217 = ADVANCED_FACE ( 'NONE', ( #1827 ), #6646, .F. ) ;
#4218 = CARTESIAN_POINT ( 'NONE',  ( 41.15000000109246514, 27.88596668178699645, 90.79316153445363113 ) ) ;
#4219 = CARTESIAN_POINT ( 'NONE',  ( 25.49999999999998934, 27.88596668178699645, 90.79316153445363113 ) ) ;
#4220 = CARTESIAN_POINT ( 'NONE',  ( 32.97500000054622404, 24.28113015263587471, 84.90069139318163138 ) ) ;
#4221 = CARTESIAN_POINT ( 'NONE',  ( 30.17500000054621978, 13.80429023900056507, 95.29460816699764791 ) ) ;
#4222 = CARTESIAN_POINT ( 'NONE',  ( 9.467847366638277862, 23.23554191946201897, 26.35090841722655952 ) ) ;
#4223 =( BOUNDED_CURVE ( )  B_SPLINE_CURVE ( 3, ( #5185, #2266, #1251, #6133 ),
 .UNSPECIFIED., .F., .F. ) 
 B_SPLINE_CURVE_WITH_KNOTS ( ( 4, 4 ),
 ( 1.570796326794896558, 3.141592653589793116 ),
 .UNSPECIFIED. ) 
 CURVE ( )  GEOMETRIC_REPRESENTATION_ITEM ( )  RATIONAL_B_SPLINE_CURVE ( ( 1.000000000000000000, 0.8047378541243649375, 0.8047378541243649375, 1.000000000000000000 ) ) 
 REPRESENTATION_ITEM ( '' )  );
#4224 = LINE ( 'NONE', #12025, #8476 ) ;
#4225 = CIRCLE ( 'NONE', #1584, 25.50000000000000711 ) ;
#4226 = ORIENTED_EDGE ( 'NONE', *, *, #3123, .T. ) ;
#4227 = CARTESIAN_POINT ( 'NONE',  ( 41.15000000109247225, 27.88596668178699645, 90.79316153445363113 ) ) ;
#4228 = ORIENTED_EDGE ( 'NONE', *, *, #2231, .T. ) ;
#4229 = DIRECTION ( 'NONE',  ( 0.000000000000000000, 1.000000000000000000, -1.039664082171044875E-15 ) ) ;
#4230 = ORIENTED_EDGE ( 'NONE', *, *, #9017, .F. ) ;
#4231 = CARTESIAN_POINT ( 'NONE',  ( -0.3289793214801078336, 10.00000000000000000, -25.00000000000000355 ) ) ;
#4232 = CARTESIAN_POINT ( 'NONE',  ( 10.00000000000000355, 20.00000000000000355, -22.91287847477919826 ) ) ;
#4233 = VECTOR ( 'NONE', #12056, 1000.000000000000000 ) ;
#4234 = DIRECTION ( 'NONE',  ( 0.000000000000000000, 1.224646799147353207E-16, 1.000000000000000000 ) ) ;
#4235 = CARTESIAN_POINT ( 'NONE',  ( 4.838449599032471404, 51.30291823734444989, 24.52740775798701378 ) ) ;
#4236 = CARTESIAN_POINT ( 'NONE',  ( -9.673562854105167474, 17.38029584746389133, 23.05303382818504332 ) ) ;
#4237 = DIRECTION ( 'NONE',  ( 0.000000000000000000, 1.000000000000000000, 0.000000000000000000 ) ) ;
#4238 = CARTESIAN_POINT ( 'NONE',  ( 6.119794236291119738, 27.93508701313207609, 20.09620109607250527 ) ) ;
#4239 = DIRECTION ( 'NONE',  ( 0.000000000000000000, 0.000000000000000000, -1.000000000000000000 ) ) ;
#4240 = FACE_OUTER_BOUND ( 'NONE', #3701, .T. ) ;
#4241 = CARTESIAN_POINT ( 'NONE',  ( -3.302172444309792620, 46.23123523635531740, -24.78206517003335208 ) ) ;
#4242 = EDGE_LOOP ( 'NONE', ( #1061, #9593, #2711, #3299 ) ) ;
#4243 = VECTOR ( 'NONE', #853, 1000.000000000000000 ) ;
#4244 = CARTESIAN_POINT ( 'NONE',  ( -9.106140955794129965, 15.85440612518673476, -26.47821835386478284 ) ) ;
#4245 = ADVANCED_FACE ( 'NONE', ( #638, #8376 ), #12247, .F. ) ;
#4246 = CARTESIAN_POINT ( 'NONE',  ( 0.6000000000000033085, 0.000000000000000000, 0.000000000000000000 ) ) ;
#4247 = CARTESIAN_POINT ( 'NONE',  ( 46.27500000054622831, 13.07298590277314254, 93.04388485072563242 ) ) ;
#4248 = CARTESIAN_POINT ( 'NONE',  ( 36.07500000054622546, 13.80429023900056507, 95.29460816699764791 ) ) ;
#4249 = CARTESIAN_POINT ( 'NONE',  ( 6.629289121864024636, 12.51307322058950611, 91.30463553460788262 ) ) ;
#4250 = CARTESIAN_POINT ( 'NONE',  ( 45.65000000109247225, 20.00000000000000355, 98.29316153445363113 ) ) ;
#4251 = CARTESIAN_POINT ( 'NONE',  ( 2.559760333650129958E-15, 55.00000000000000000, 21.00000000000000000 ) ) ;
#4252 = CARTESIAN_POINT ( 'NONE',  ( 27.27500000054622475, 27.65831843345427998, 90.79316153445363113 ) ) ;
#4253 = VERTEX_POINT ( 'NONE', #1648 ) ;
#4254 = DIRECTION ( 'NONE',  ( 0.000000000000000000, 0.000000000000000000, -1.000000000000000000 ) ) ;
#4255 = ORIENTED_EDGE ( 'NONE', *, *, #5368, .F. ) ;
#4256 = ORIENTED_EDGE ( 'NONE', *, *, #5253, .F. ) ;
#4257 = CARTESIAN_POINT ( 'NONE',  ( 38.89999999999999147, 17.56310227825319359, 83.29316153445364534 ) ) ;
#4258 = VERTEX_POINT ( 'NONE', #12306 ) ;
#4259 = CARTESIAN_POINT ( 'NONE',  ( 29.57500000054621836, 26.19570976099943849, 95.29460816699764791 ) ) ;
#4260 = DIRECTION ( 'NONE',  ( 0.000000000000000000, 0.000000000000000000, -1.000000000000000000 ) ) ;
#4261 = CARTESIAN_POINT ( 'NONE',  ( -2.065290181436918893, 45.44356257902996532, -27.92413535551499848 ) ) ;
#4262 = SHAPE_REPRESENTATION ( 'MAS-314', ( #5955, #10806, #6764, #12231, #4938, #9808, #8381, #10603, #11421, #11831, #683, #1501, #5761, #12036, #11018, #8587 ), #7988 ) ;
#4263 = CARTESIAN_POINT ( 'NONE',  ( 38.27500000054622831, 13.07298590277314254, 93.04388485072563242 ) ) ;
#4264 = CARTESIAN_POINT ( 'NONE',  ( 36.29999999999997584, 13.62011893735971135, 95.42841645007781892 ) ) ;
#4265 = ADVANCED_FACE ( 'NONE', ( #3607, #7485 ), #127, .T. ) ;
#4266 = CARTESIAN_POINT ( 'NONE',  ( 43.47500000054623115, 26.19570976099943493, 95.29460816699764791 ) ) ;
#4267 = ORIENTED_EDGE ( 'NONE', *, *, #11999, .T. ) ;
#4268 = CARTESIAN_POINT ( 'NONE',  ( 27.45000000109246585, 24.40838939219354842, 96.86078899226572503 ) ) ;
#4269 = CARTESIAN_POINT ( 'NONE',  ( -10.00000000000000355, 20.00000000000000355, 22.91287847477919826 ) ) ;
#4270 = ORIENTED_EDGE ( 'NONE', *, *, #6526, .F. ) ;
#4271 = CARTESIAN_POINT ( 'NONE',  ( -10.00000000000000533, 20.32816415950047073, 26.15339366124404208 ) ) ;
#4272 = EDGE_LOOP ( 'NONE', ( #5387, #7660, #330, #7515 ) ) ;
#4273 = DIRECTION ( 'NONE',  ( 1.000000000000000000, -0.000000000000000000, -0.000000000000000000 ) ) ;
#4274 = PRODUCT_DEFINITION_SHAPE ( 'NONE', 'NONE',  #12552 ) ;
#4275 = CARTESIAN_POINT ( 'NONE',  ( 40.65000000109246514, 20.00000000000000355, 83.29316153445364534 ) ) ;
#4276 = CARTESIAN_POINT ( 'NONE',  ( 32.07500000054623257, 13.80429023900056507, 95.29460816699764791 ) ) ;
#4277 = CARTESIAN_POINT ( 'NONE',  ( 22.87500000054622618, 20.00000000000000355, 83.50966788445364841 ) ) ;
#4278 = EDGE_CURVE ( 'NONE', #169, #9642, #5833, .T. ) ;
#4279 = CARTESIAN_POINT ( 'NONE',  ( 27.49999999999999645, 20.00000000000000355, 188.9999999999999716 ) ) ;
#4280 = FACE_OUTER_BOUND ( 'NONE', #11089, .T. ) ;
#4281 = VERTEX_POINT ( 'NONE', #12490 ) ;
#4282 = AXIS2_PLACEMENT_3D ( 'NONE', #4804, #8669, #12539 ) ;
#4283 = CARTESIAN_POINT ( 'NONE',  ( 43.55000000109246372, 22.43689772174679575, 98.29316153445363113 ) ) ;
#4284 = SURFACE_SIDE_STYLE ('',( #6251 ) ) ;
#4285 = ORIENTED_EDGE ( 'NONE', *, *, #10468, .F. ) ;
#4286 = DIRECTION ( 'NONE',  ( 1.000000000000000000, 0.000000000000000000, 0.000000000000000000 ) ) ;
#4287 = EDGE_CURVE ( 'NONE', #12540, #6613, #4198, .T. ) ;
#4288 = ORIENTED_EDGE ( 'NONE', *, *, #7758, .T. ) ;
#4289 = CARTESIAN_POINT ( 'NONE',  ( -4.441326820874226478, 11.03441940688963108, -24.60408056175351987 ) ) ;
#4290 = CARTESIAN_POINT ( 'NONE',  ( -4.448741964560915640, 28.96190946584970405, 24.60274125495980613 ) ) ;
#4291 = DIRECTION ( 'NONE',  ( 1.000000000000000000, -0.000000000000000000, -0.000000000000000000 ) ) ;
#4292 = ADVANCED_BREP_SHAPE_REPRESENTATION ( '', ( #1830, #9021 ), #1096 ) ;
#4293 = EDGE_CURVE ( 'NONE', #4576, #2177, #4225, .T. ) ;
#4294 = SURFACE_SIDE_STYLE ('',( #2448 ) ) ;
#4295 = CARTESIAN_POINT ( 'NONE',  ( -0.3301927727158289749, 10.00000000000000000, 25.00000000000000355 ) ) ;
#4296 = CARTESIAN_POINT ( 'NONE',  ( 20.27158385259951956, 18.00000000000000355, 169.9999999999999716 ) ) ;
#4297 = CARTESIAN_POINT ( 'NONE',  ( -7.945225341866328783, 13.89296426715405453, 19.44295823276161173 ) ) ;
#4298 = CARTESIAN_POINT ( 'NONE',  ( -8.486085304528891982, 14.69985328301606842, 26.68374292945578574 ) ) ;
#4299 = CARTESIAN_POINT ( 'NONE',  ( 7.520704636030203893, 26.59870071877557507, -19.60835093631877513 ) ) ;
#4300 = CARTESIAN_POINT ( 'NONE',  ( -6.999999999999999112, 69.50000000000000000, 146.8533255156881978 ) ) ;
#4301 = ORIENTED_EDGE ( 'NONE', *, *, #3563, .T. ) ;
#4302 = CARTESIAN_POINT ( 'NONE',  ( -8.655424981280289032, 14.98103440478909398, -26.62912044845977988 ) ) ;
#4303 = CARTESIAN_POINT ( 'NONE',  ( 3.052604782738682854, 46.02637368922790984, 24.81445626415020200 ) ) ;
#4304 = LINE ( 'NONE', #8181, #2367 ) ;
#4305 = CARTESIAN_POINT ( 'NONE',  ( 45.87500000054622973, 20.00000000000000355, 98.07665518445361386 ) ) ;
#4306 = CARTESIAN_POINT ( 'NONE',  ( 24.57500000054622902, 15.71886984736413773, 84.90069139318163138 ) ) ;
#4307 = CARTESIAN_POINT ( 'NONE',  ( 9.959687983327881966, 18.97177336558172911, 83.34667569529023012 ) ) ;
#4308 = AXIS2_PLACEMENT_3D ( 'NONE', #5012, #3989, #11606 ) ;
#4309 = CARTESIAN_POINT ( 'NONE',  ( 33.19999999999998863, 24.40838939219355197, 84.72553407664153724 ) ) ;
#4310 = DIRECTION ( 'NONE',  ( 1.000000000000000000, -0.000000000000000000, -0.000000000000000000 ) ) ;
#4311 = CARTESIAN_POINT ( 'NONE',  ( 24.87500000054622618, 22.36655054427230382, 83.50966788445364841 ) ) ;
#4312 = ORIENTED_EDGE ( 'NONE', *, *, #2844, .T. ) ;
#4313 = PLANE ( 'NONE',  #11975 ) ;
#4314 = EDGE_CURVE ( 'NONE', #4704, #3374, #6258, .T. ) ;
#4315 = B_SPLINE_CURVE_WITH_KNOTS ( 'NONE', 3,
 ( #5302, #3389, #7132, #10946, #9172, #4222, #417, #11006, #4464, #10240, #6314, #8279, #8343, #6374, #2319, #6186, #1489, #10061, #12148, #10181, #479, #1372, #5365, #4346 ),
 .UNSPECIFIED., .F., .F.,
 ( 4, 2, 2, 2, 2, 2, 2, 2, 2, 2, 2, 4 ),
 ( 0.000000000000000000, 0.001970972387426263902, 0.002956458581139390866, 0.003941944774852517396, 0.005912917162278783466, 0.006898403355991919103, 0.007883889549705055608, 0.009854861937131328617, 0.01182583432455759989, 0.01281132051827073466, 0.01379680671198387117, 0.01576777909941014244 ),
 .UNSPECIFIED. ) ;
#4316 = DIRECTION ( 'NONE',  ( 0.000000000000000000, 0.000000000000000000, 1.000000000000000000 ) ) ;
#4317 = ORIENTED_EDGE ( 'NONE', *, *, #7463, .F. ) ;
#4318 =( REPRESENTATION_RELATIONSHIP ('NONE','NONE', #4262, #3370 ) REPRESENTATION_RELATIONSHIP_WITH_TRANSFORMATION ( #10706 )SHAPE_REPRESENTATION_RELATIONSHIP( ) );
#4319 = VECTOR ( 'NONE', #6959, 1000.000000000000000 ) ;
#4320 = CARTESIAN_POINT ( 'NONE',  ( 29.17500000054622333, 26.19570976099943849, 86.29171490190961435 ) ) ;
#4321 = DIRECTION ( 'NONE',  ( 0.000000000000000000, 0.000000000000000000, 1.000000000000000000 ) ) ;
#4322 = CARTESIAN_POINT ( 'NONE',  ( 44.57500000054622546, 15.71886984736413773, 84.90069139318163138 ) ) ;
#4323 = CARTESIAN_POINT ( 'NONE',  ( 32.47500000054621694, 13.07298590277314432, 88.54243821818161564 ) ) ;
#4324 = CARTESIAN_POINT ( 'NONE',  ( 37.39999999999999147, 27.13292387221364876, 88.47553407664153724 ) ) ;
#4325 = CARTESIAN_POINT ( 'NONE',  ( 44.07500000054623968, 13.80429023900056507, 95.29460816699764791 ) ) ;
#4326 = ORIENTED_EDGE ( 'NONE', *, *, #5218, .F. ) ;
#4327 = VECTOR ( 'NONE', #12405, 1000.000000000000000 ) ;
#4328 = CARTESIAN_POINT ( 'NONE',  ( 22.55000000109246017, 17.56310227825321135, 83.29316153445363113 ) ) ;
#4329 = CARTESIAN_POINT ( 'NONE',  ( 0.000000000000000000, -2.342598717236911821, -4.057499999999996554 ) ) ;
#4330 = ORIENTED_EDGE ( 'NONE', *, *, #647, .F. ) ;
#4331 = CARTESIAN_POINT ( 'NONE',  ( -6.848757607247366153, 27.29383130221564713, 27.15051995320520462 ) ) ;
#4332 =( GEOMETRIC_REPRESENTATION_CONTEXT ( 3 ) GLOBAL_UNCERTAINTY_ASSIGNED_CONTEXT ( ( #11603 ) ) GLOBAL_UNIT_ASSIGNED_CONTEXT ( ( #5278, #1283, #10098 ) ) REPRESENTATION_CONTEXT ( 'NONE', 'WORKASPACE' ) );
#4333 = ORIENTED_EDGE ( 'NONE', *, *, #12357, .F. ) ;
#4334 = FACE_OUTER_BOUND ( 'NONE', #1066, .T. ) ;
#4335 = CARTESIAN_POINT ( 'NONE',  ( 0.000000000000000000, 5.839897972853065333, -6.938893903907228378E-15 ) ) ;
#4336 = EDGE_CURVE ( 'NONE', #9180, #8859, #5076, .T. ) ;
#4337 = B_SPLINE_CURVE_WITH_KNOTS ( 'NONE', 3,
 ( #8578, #2680, #775, #3686, #8891, #8007, #11808, #4001, #9849, #143, #2166, #8823, #6105, #8072, #10722, #7046, #4132, #6038 ),
 .UNSPECIFIED., .F., .F.,
 ( 4, 2, 2, 2, 2, 2, 2, 2, 4 ),
 ( 5.188175463412582976E-20, 0.0009797360301013575360, 0.001959472060202715072, 0.002939208090304072825, 0.003918944120405430144, 0.004898680150506787463, 0.005878416180608145650, 0.006858152210709502969, 0.007837888240810860288 ),
 .UNSPECIFIED. ) ;
#4338 = DIRECTION ( 'NONE',  ( 0.000000000000000000, 0.000000000000000000, -1.000000000000000000 ) ) ;
#4339 = SHAPE_REPRESENTATION ( 'Bolt-Mounted Retaining Cylinder', ( #9021 ), #5775 ) ;
#4340 = DIRECTION ( 'NONE',  ( 1.000000000000000000, -0.000000000000000000, -0.000000000000000000 ) ) ;
#4341 = VECTOR ( 'NONE', #3752, 1000.000000000000000 ) ;
#4342 = CARTESIAN_POINT ( 'NONE',  ( 26.97500000054622760, 24.28113015263587471, 84.90069139318163138 ) ) ;
#4343 = CARTESIAN_POINT ( 'NONE',  ( 27.17500000054621978, 26.19570976099943493, 86.29171490190961435 ) ) ;
#4344 = VECTOR ( 'NONE', #3572, 1000.000000000000000 ) ;
#4345 = EDGE_CURVE ( 'NONE', #1748, #5412, #404, .T. ) ;
#4346 = CARTESIAN_POINT ( 'NONE',  ( 3.429011038972528284E-15, 30.00000000000001066, 28.00000000000000355 ) ) ;
#4347 = DIRECTION ( 'NONE',  ( 0.000000000000000000, 0.000000000000000000, -1.000000000000000000 ) ) ;
#4348 = ORIENTED_EDGE ( 'NONE', *, *, #4417, .F. ) ;
#4349 = CARTESIAN_POINT ( 'NONE',  ( 41.75000000109247367, 17.56310227825320425, 98.29316153445363113 ) ) ;
#4350 = DIRECTION ( 'NONE',  ( 0.000000000000000000, -1.000000000000000000, 1.295896757998781572E-15 ) ) ;
#4351 = ORIENTED_EDGE ( 'NONE', *, *, #261, .F. ) ;
#4352 = DIRECTION ( 'NONE',  ( 0.000000000000000000, 0.000000000000000000, -1.000000000000000000 ) ) ;
#4353 = VERTEX_POINT ( 'NONE', #11923 ) ;
#4354 = AXIS2_PLACEMENT_3D ( 'NONE', #8479, #8663, #6507 ) ;
#4355 = CARTESIAN_POINT ( 'NONE',  ( 3.304769568038884664, 53.76613650905855479, 20.73964112051737274 ) ) ;
#4356 = DIRECTION ( 'NONE',  ( -1.000000000000000000, -0.000000000000000000, -0.000000000000000000 ) ) ;
#4357 = CARTESIAN_POINT ( 'NONE',  ( 6.999999999999964473, 20.00000000000000355, -70.00000000000000000 ) ) ;
#4358 = EDGE_CURVE ( 'NONE', #8530, #918, #11030, .T. ) ;
#4359 = CARTESIAN_POINT ( 'NONE',  ( -1.325835098444672733, 10.08270123135439711, 24.96701611100131402 ) ) ;
#4360 = CARTESIAN_POINT ( 'NONE',  ( 6.000000000000000000, -5.839897972853060892, 7.806255641895631925E-15 ) ) ;
#4361 = CONICAL_SURFACE ( 'NONE', #8417, 10.00000000000000355, 0.7853981633974520538 ) ;
#4362 = DIRECTION ( 'NONE',  ( 1.000000000000000000, 0.000000000000000000, 0.000000000000000000 ) ) ;
#4363 = DIRECTION ( 'NONE',  ( 0.000000000000000000, 0.000000000000000000, 1.000000000000000000 ) ) ;
#4364 = CARTESIAN_POINT ( 'NONE',  ( 9.983143436873248788, 20.66859359106200955, 22.92025639428880623 ) ) ;
#4365 = CARTESIAN_POINT ( 'NONE',  ( -20.00000000000001776, 20.00000000000000000, 137.5000000000000000 ) ) ;
#4366 = ORIENTED_EDGE ( 'NONE', *, *, #6755, .F. ) ;
#4367 = EDGE_CURVE ( 'NONE', #2044, #4011, #12050, .T. ) ;
#4368 = DIRECTION ( 'NONE',  ( 1.000000000000000000, 0.000000000000000000, 0.000000000000000000 ) ) ;
#4369 = CARTESIAN_POINT ( 'NONE',  ( 0.3299754220453550713, 55.00000000000001421, 25.00000000000000000 ) ) ;
#4370 = CARTESIAN_POINT ( 'NONE',  ( 41.97500000054623115, 17.63344945572769973, 98.07665518445361386 ) ) ;
#4371 = CARTESIAN_POINT ( 'NONE',  ( 27.97500000054623115, 15.71886984736413417, 96.68563167572563088 ) ) ;
#4372 = CARTESIAN_POINT ( 'NONE',  ( 36.99999999999995026, 0.000000000000000000, 69.99999999999998579 ) ) ;
#4373 = DIRECTION ( 'NONE',  ( 0.000000000000000000, -0.000000000000000000, -1.000000000000000000 ) ) ;
#4374 = DIRECTION ( 'NONE',  ( 1.000000000000000000, 0.000000000000000000, 0.000000000000000000 ) ) ;
#4375 = FACE_OUTER_BOUND ( 'NONE', #609, .T. ) ;
#4376 = ORIENTED_EDGE ( 'NONE', *, *, #9788, .T. ) ;
#4377 = CARTESIAN_POINT ( 'NONE',  ( 27.49999999999999645, 20.00000000000000355, 99.99999999999997158 ) ) ;
#4378 = CARTESIAN_POINT ( 'NONE',  ( 38.79999999999999005, 15.59161060780646046, 84.72553407664153724 ) ) ;
#4379 = ORIENTED_EDGE ( 'NONE', *, *, #6506, .F. ) ;
#4380 = CARTESIAN_POINT ( 'NONE',  ( 30.27500000054622475, 13.07298590277314254, 93.04388485072563242 ) ) ;
#4381 = CYLINDRICAL_SURFACE ( 'NONE', #3696, 9.000000000000000000 ) ;
#4382 = CARTESIAN_POINT ( 'NONE',  ( 44.77500000054623541, 20.00000000000000355, 83.50966788445364841 ) ) ;
#4383 = CARTESIAN_POINT ( 'NONE',  ( 36.07500000054622546, 15.71886984736413417, 96.68563167572563088 ) ) ;
#4384 = CARTESIAN_POINT ( 'NONE',  ( 36.59999999999998721, 12.86707612778636012, 88.47553407664152303 ) ) ;
#4385 = CARTESIAN_POINT ( 'NONE',  ( 4.444397983376138228, 28.96407317687630822, 24.60352964329958070 ) ) ;
#4386 = CARTESIAN_POINT ( 'NONE',  ( 48.57500000054623257, 15.71886984736413773, 84.90069139318163138 ) ) ;
#4387 = ORIENTED_EDGE ( 'NONE', *, *, #9879, .F. ) ;
#4388 = CARTESIAN_POINT ( 'NONE',  ( 24.55000000109246017, 17.56310227825321135, 83.29316153445363113 ) ) ;
#4389 = CARTESIAN_POINT ( 'NONE',  ( -2.217326200926027724, 45.51555228448187762, 24.90189708455264395 ) ) ;
#4390 = TOROIDAL_SURFACE ( 'NONE', #12486, 8.400000000000000355, 0.5999999999999999778 ) ;
#4391 = ORIENTED_EDGE ( 'NONE', *, *, #11469, .F. ) ;
#4392 = CARTESIAN_POINT ( 'NONE',  ( -9.674652806887369394, 22.61498962668658308, 26.27585132995591621 ) ) ;
#4393 = ORIENTED_EDGE ( 'NONE', *, *, #6827, .T. ) ;
#4394 = CARTESIAN_POINT ( 'NONE',  ( 10.40000000000000036, 6.123233995736767268E-16, -5.000000000000000888 ) ) ;
#4395 = DIRECTION ( 'NONE',  ( 0.000000000000000000, -0.4999999999999989453, 0.8660254037844393737 ) ) ;
#4396 = CARTESIAN_POINT ( 'NONE',  ( 36.65000000109245804, 20.00000000000000355, 83.29316153445364534 ) ) ;
#4397 = DIRECTION ( 'NONE',  ( 0.000000000000000000, 0.000000000000000000, 1.000000000000000000 ) ) ;
#4398 = CIRCLE ( 'NONE', #954, 5.057500000000000107 ) ;
#4399 = ADVANCED_FACE ( 'NONE', ( #1456 ), #2340, .T. ) ;
#4400 = CARTESIAN_POINT ( 'NONE',  ( 26.57500000054622902, 15.71886984736413773, 84.90069139318163138 ) ) ;
#4401 = CARTESIAN_POINT ( 'NONE',  ( 23.27500000054622475, 26.92701409722686634, 88.54243821818162985 ) ) ;
#4402 = CARTESIAN_POINT ( 'NONE',  ( 19.93750000027310421, 20.00000000000000355, 98.18490835945361539 ) ) ;
#4403 = CARTESIAN_POINT ( 'NONE',  ( 5.000000000000000000, -2.342598717236902051, 4.057500000000004547 ) ) ;
#4404 = ORIENTED_EDGE ( 'NONE', *, *, #7849, .F. ) ;
#4405 = CARTESIAN_POINT ( 'NONE',  ( 45.55000000109247082, 22.43689772174679575, 98.29316153445363113 ) ) ;
#4406 = FILL_AREA_STYLE_COLOUR ( '', #10497 ) ;
#4407 = EDGE_LOOP ( 'NONE', ( #12, #12317, #4769, #3746, #284 ) ) ;
#4408 = CARTESIAN_POINT ( 'NONE',  ( 30.35000000109246088, 13.62011893735970958, 86.15790661882942914 ) ) ;
#4409 = ORIENTED_EDGE ( 'NONE', *, *, #8138, .F. ) ;
#4410 = AXIS2_PLACEMENT_3D ( 'NONE', #2373, #10940, #3450 ) ;
#4411 = LINE ( 'NONE', #10364, #10125 ) ;
#4412 = CARTESIAN_POINT ( 'NONE',  ( 7.537524037383855458, 13.39612119810769819, -23.84148986838564710 ) ) ;
#4413 = DIRECTION ( 'NONE',  ( 0.000000000000000000, 0.000000000000000000, -1.000000000000000000 ) ) ;
#4414 = VECTOR ( 'NONE', #10357, 1000.000000000000000 ) ;
#4415 = FACE_OUTER_BOUND ( 'NONE', #1523, .T. ) ;
#4416 = DIRECTION ( 'NONE',  ( -1.000000000000000000, 0.000000000000000000, 0.000000000000000000 ) ) ;
#4417 = EDGE_CURVE ( 'NONE', #11047, #6436, #3583, .T. ) ;
#4418 = CARTESIAN_POINT ( 'NONE',  ( -9.102716943808436767, 15.84719902056293250, 18.92511310367350319 ) ) ;
#4419 = CARTESIAN_POINT ( 'NONE',  ( -6.597987972726388151, 12.47858281773167199, 27.21273137650036134 ) ) ;
#4420 = CARTESIAN_POINT ( 'NONE',  ( 0.6000000000000033085, 0.000000000000000000, 0.000000000000000000 ) ) ;
#4421 = CARTESIAN_POINT ( 'NONE',  ( -2.221358530307614654, 54.49149874209361144, 24.90297606857491175 ) ) ;
#4422 = ORIENTED_EDGE ( 'NONE', *, *, #1524, .F. ) ;
#4423 = AXIS2_PLACEMENT_3D ( 'NONE', #1639, #10445, #10510 ) ;
#4424 = EDGE_CURVE ( 'NONE', #9969, #11906, #254, .T. ) ;
#4425 = DIRECTION ( 'NONE',  ( -1.000000000000000000, 0.000000000000000000, 0.000000000000000000 ) ) ;
#4426 = DIRECTION ( 'NONE',  ( -1.000000000000000000, -0.000000000000000000, -0.000000000000000000 ) ) ;
#4427 = CARTESIAN_POINT ( 'NONE',  ( 38.67500000054622689, 15.71886984736413773, 84.90069139318163138 ) ) ;
#4428 = CARTESIAN_POINT ( 'NONE',  ( 27.77500000054622831, 20.00000000000000355, 98.07665518445361386 ) ) ;
#4429 = EDGE_CURVE ( 'NONE', #8586, #10212, #10905, .T. ) ;
#4430 = VECTOR ( 'NONE', #12347, 1000.000000000000000 ) ;
#4431 = CARTESIAN_POINT ( 'NONE',  ( 9.796987274755800001, 17.98000013482726089, 83.56587684317791798 ) ) ;
#4432 = CARTESIAN_POINT ( 'NONE',  ( 45.15000000109246514, 27.88596668178699645, 90.79316153445363113 ) ) ;
#4433 = CARTESIAN_POINT ( 'NONE',  ( 35.99999999999999289, 20.00000000000000355, 98.29316153445363113 ) ) ;
#4434 = FACE_OUTER_BOUND ( 'NONE', #73, .T. ) ;
#4435 = EDGE_CURVE ( 'NONE', #3380, #7100, #5240, .T. ) ;
#4436 = CLOSED_SHELL ( 'NONE', ( #11482, #7353, #2728, #10960, #6407, #1023, #5569, #1609, #7333, #2767, #10453, #12495, #1914, #10001, #6181, #6288, #635, #10769, #8835, #8056, #8860, #11266, #4721, #4399, #8066, #4081, #11840 ) ) ;
#4437 = ORIENTED_EDGE ( 'NONE', *, *, #5792, .F. ) ;
#4438 = DIRECTION ( 'NONE',  ( 1.000000000000000000, 0.000000000000000000, -0.000000000000000000 ) ) ;
#4439 = ORIENTED_EDGE ( 'NONE', *, *, #10182, .F. ) ;
#4440 = CARTESIAN_POINT ( 'NONE',  ( 0.6000000000000033085, 0.000000000000000000, 8.400000000000000355 ) ) ;
#4441 = ADVANCED_FACE ( 'NONE', ( #9874 ), #1186, .F. ) ;
#4442 =( NAMED_UNIT ( * ) SI_UNIT ( $, .STERADIAN. ) SOLID_ANGLE_UNIT ( ) );
#4443 = AXIS2_PLACEMENT_3D ( 'NONE', #1822, #814, #10448 ) ;
#4444 = CIRCLE ( 'NONE', #7080, 23.49999999999999289 ) ;
#4445 = CARTESIAN_POINT ( 'NONE',  ( 31.07500000054622546, 24.28113015263587471, 84.90069139318163138 ) ) ;
#4446 = CARTESIAN_POINT ( 'NONE',  ( -3.976827824928235611, 53.04822971330205661, -27.71675544712706696 ) ) ;
#4447 = CARTESIAN_POINT ( 'NONE',  ( 44.27500000054622120, 12.34168156654572357, 90.79316153445363113 ) ) ;
#4448 = CARTESIAN_POINT ( 'NONE',  ( 30.97500000054622760, 22.36655054427230382, 83.50966788445364841 ) ) ;
#4449 = CARTESIAN_POINT ( 'NONE',  ( 37.79999999999998295, 24.40838939219354842, 96.86078899226572503 ) ) ;
#4450 = CARTESIAN_POINT ( 'NONE',  ( 10.00000000000000888, 20.33378987232122981, 22.91287847477920536 ) ) ;
#4451 = CARTESIAN_POINT ( 'NONE',  ( 40.37500000054622973, 13.07298590277314432, 88.54243821818161564 ) ) ;
#4452 = ORIENTED_EDGE ( 'NONE', *, *, #1262, .T. ) ;
#4453 = CARTESIAN_POINT ( 'NONE',  ( 45.97500000054623115, 15.71886984736413417, 96.68563167572563088 ) ) ;
#4454 = CARTESIAN_POINT ( 'NONE',  ( -4.999999999999999112, 49.67330453822126657, 24.49489742783177348 ) ) ;
#4455 = ORIENTED_EDGE ( 'NONE', *, *, #9568, .F. ) ;
#4456 = DIRECTION ( 'NONE',  ( 0.000000000000000000, 0.000000000000000000, -1.000000000000000000 ) ) ;
#4457 = ORIENTED_EDGE ( 'NONE', *, *, #9017, .T. ) ;
#4458 = DIRECTION ( 'NONE',  ( -0.000000000000000000, -1.000000000000000000, -0.000000000000000000 ) ) ;
#4459 = FACE_OUTER_BOUND ( 'NONE', #10560, .T. ) ;
#4460 = DIRECTION ( 'NONE',  ( 1.000000000000000000, 0.000000000000000000, 0.000000000000000000 ) ) ;
#4461 = CARTESIAN_POINT ( 'NONE',  ( 31.95000000109245875, 13.62011893735970958, 95.42841645007781892 ) ) ;
#4462 = CARTESIAN_POINT ( 'NONE',  ( 26.37500000054622973, 13.07298590277314432, 88.54243821818161564 ) ) ;
#4463 = CARTESIAN_POINT ( 'NONE',  ( 22.27500000054622120, 13.07298590277314254, 93.04388485072563242 ) ) ;
#4464 = CARTESIAN_POINT ( 'NONE',  ( 8.669775631709102370, 25.02591811617444151, 26.62666687084030315 ) ) ;
#4465 = CARTESIAN_POINT ( 'NONE',  ( -4.838865259365938698, 48.69895664399926005, 24.52732495089485099 ) ) ;
#4466 = ORIENTED_EDGE ( 'NONE', *, *, #6134, .F. ) ;
#4467 = CARTESIAN_POINT ( 'NONE',  ( 45.15000000109245804, 27.88596668178699645, 90.79316153445363113 ) ) ;
#4468 = CARTESIAN_POINT ( 'NONE',  ( 3.651743720672741667, 53.41923203171982237, -24.73212923346887848 ) ) ;
#4469 = ORIENTED_EDGE ( 'NONE', *, *, #4882, .F. ) ;
#4470 = CARTESIAN_POINT ( 'NONE',  ( 0.000000000000000000, 20.00000000000000355, -66.99999999999998579 ) ) ;
#4471 = AXIS2_PLACEMENT_3D ( 'NONE', #12367, #10392, #1704 ) ;
#4472 = EDGE_CURVE ( 'NONE', #2741, #5074, #11928, .T. ) ;
#4473 = ORIENTED_EDGE ( 'NONE', *, *, #11166, .F. ) ;
#4474 = EDGE_CURVE ( 'NONE', #2895, #136, #8115, .T. ) ;
#4475 = CARTESIAN_POINT ( 'NONE',  ( 90.00000000000000000, 5.616230220889762438E-16, -4.171999999999999709 ) ) ;
#4476 = B_SPLINE_CURVE_WITH_KNOTS ( 'NONE', 3,
 ( #12047, #8054, #6147, #7089, #10831, #11028, #2278, #9893, #1453, #8240, #9068, #4241, #7989, #4110, #11983, #6208, #3347, #1390, #7214, #502 ),
 .UNSPECIFIED., .F., .F.,
 ( 4, 2, 2, 2, 2, 2, 2, 2, 2, 4 ),
 ( 0.007837888240810860288, 0.008817134455640363022, 0.009796380670469867491, 0.01028600377788460932, 0.01077562688529935114, 0.01175487310012885388, 0.01273411931495835661, 0.01371336552978785761, 0.01469261174461736208, 0.01567185795944686308 ),
 .UNSPECIFIED. ) ;
#4477 = CARTESIAN_POINT ( 'NONE',  ( 3.246557057937244029, 10.51899376542992925, -24.79585947768713439 ) ) ;
#4478 = CYLINDRICAL_SURFACE ( 'NONE', #11827, 7.499999999999992895 ) ;
#4479 = CONICAL_SURFACE ( 'NONE', #6106, 10.00000000000000355, 0.7853981633974520538 ) ;
#4480 = CARTESIAN_POINT ( 'NONE',  ( 12.00000000000000178, 9.000000000000000000, 0.000000000000000000 ) ) ;
#4481 = CARTESIAN_POINT ( 'NONE',  ( -3.246935905771412667, 10.51876153604172970, 24.79592758899451255 ) ) ;
#4482 = LINE ( 'NONE', #2389, #7058 ) ;
#4483 = CARTESIAN_POINT ( 'NONE',  ( 6.000000000000000000, 5.839897972853065333, -6.938893903907228378E-15 ) ) ;
#4484 = CARTESIAN_POINT ( 'NONE',  ( 27.49999999999999645, 20.00000000000000355, 170.0000119999999697 ) ) ;
#4485 = DIRECTION ( 'NONE',  ( 0.000000000000000000, -1.110768649713241713E-15, -1.000000000000000000 ) ) ;
#4486 = CARTESIAN_POINT ( 'NONE',  ( -4.246666789336575931, 52.64435674096336015, 24.63684932116156645 ) ) ;
#4487 = ORIENTED_EDGE ( 'NONE', *, *, #9521, .T. ) ;
#4488 = CARTESIAN_POINT ( 'NONE',  ( 3.764226701178052803, 46.69296989397847852, 24.71608072572789538 ) ) ;
#4489 = EDGE_CURVE ( 'NONE', #5074, #10297, #5524, .T. ) ;
#4490 = B_SPLINE_CURVE_WITH_KNOTS ( 'NONE', 3,
 ( #3116, #10856, #1759, #815, #1953, #3792, #7795, #2013, #5642, #8617, #9575, #122, #11599, #10513, #1074, #11667, #11472, #3919 ),
 .UNSPECIFIED., .F., .F.,
 ( 4, 2, 2, 2, 2, 2, 2, 2, 4 ),
 ( 0.02349634876194046582, 0.02447473093966404806, 0.02545311311738762683, 0.02643149529511120907, 0.02740987747283479131, 0.02838825965055837355, 0.02936664182828195579, 0.03034502400600553804, 0.03132340618372912028 ),
 .UNSPECIFIED. ) ;
#4491 = DIRECTION ( 'NONE',  ( 1.000000000000000000, -0.000000000000000000, -0.000000000000000000 ) ) ;
#4492 = CARTESIAN_POINT ( 'NONE',  ( 36.97500000054623115, 22.36655054427230382, 83.50966788445364841 ) ) ;
#4493 = CARTESIAN_POINT ( 'NONE',  ( 24.97500000054622760, 24.28113015263587471, 84.90069139318163138 ) ) ;
#4494 = CARTESIAN_POINT ( 'NONE',  ( 7.619081503294689028, 13.51451987764450990, 94.58903075352336032 ) ) ;
#4495 = CARTESIAN_POINT ( 'NONE',  ( 3.052604782738682854, 46.02637368922790984, 24.81445626415020200 ) ) ;
#4496 = ADVANCED_FACE ( 'NONE', ( #9684 ), #11709, .F. ) ;
#4497 = CARTESIAN_POINT ( 'NONE',  ( -31.74999999999995737, 1.102182119232617714E-15, -9.000000000000000000 ) ) ;
#4498 = PLANE ( 'NONE',  #590 ) ;
#4499 = ORIENTED_EDGE ( 'NONE', *, *, #1677, .T. ) ;
#4500 = PLANE ( 'NONE',  #2443 ) ;
#4501 = ORIENTED_EDGE ( 'NONE', *, *, #5303, .F. ) ;
#4502 = CARTESIAN_POINT ( 'NONE',  ( 33.79382810696422013, 14.62220435867159551, 151.2938281069642130 ) ) ;
#4503 = B_SPLINE_CURVE_WITH_KNOTS ( 'NONE', 3,
 ( #8903, #10867, #9735, #6051, #9924, #3955, #1233, #1051, #7829, #6301, #11118, #10111, #10171, #12075, #1541, #5228, #8207, #11951, #11181, #1478, #1422, #5168, #3315, #12011, #6237, #6361 ),
 .UNSPECIFIED., .F., .F.,
 ( 4, 2, 2, 2, 2, 2, 2, 2, 2, 2, 2, 2, 4 ),
 ( 0.01580376012220196039, 0.01679085241551835084, 0.01777794470883474129, 0.01975212929546752219, 0.02172631388210030656, 0.02271340617541669701, 0.02370049846873308746, 0.02567468305536586837, 0.02666177534868225882, 0.02764886764199864927, 0.02962305222863143364, 0.03061014452194782409, 0.03159723681526421801 ),
 .UNSPECIFIED. ) ;
#4504 = CARTESIAN_POINT ( 'NONE',  ( 34.57500000054622546, 13.80429023900056684, 86.29171490190961435 ) ) ;
#4505 = CARTESIAN_POINT ( 'NONE',  ( 27.25000000109246656, 27.13292387221364876, 93.11078899226573924 ) ) ;
#4506 = CARTESIAN_POINT ( 'NONE',  ( 47.67500000054622689, 22.36655054427230027, 98.07665518445361386 ) ) ;
#4507 = CARTESIAN_POINT ( 'NONE',  ( 34.47500000054622404, 13.07298590277314432, 88.54243821818161564 ) ) ;
#4508 = CARTESIAN_POINT ( 'NONE',  ( 34.59999999999999432, 12.86707612778636012, 88.47553407664152303 ) ) ;
#4509 = EDGE_CURVE ( 'NONE', #10081, #12073, #8074, .T. ) ;
#4510 = CARTESIAN_POINT ( 'NONE',  ( 0.000000000000000000, -5.839897972853060892, 7.806255641895631925E-15 ) ) ;
#4511 = CARTESIAN_POINT ( 'NONE',  ( 38.47500000054621694, 13.80429023900056684, 86.29171490190961435 ) ) ;
#4512 = ORIENTED_EDGE ( 'NONE', *, *, #7204, .T. ) ;
#4513 = CARTESIAN_POINT ( 'NONE',  ( 20.45000000109246585, 15.59161060780646046, 84.72553407664153724 ) ) ;
#4514 = LINE ( 'NONE', #3498, #2838 ) ;
#4515 = ORIENTED_EDGE ( 'NONE', *, *, #3310, .T. ) ;
#4516 = CARTESIAN_POINT ( 'NONE',  ( -6.613224532456894345, 27.52898668827616646, -27.21194102765744560 ) ) ;
#4517 = ORIENTED_EDGE ( 'NONE', *, *, #1269, .T. ) ;
#4518 = CIRCLE ( 'NONE', #7552, 5.035999999999999588 ) ;
#4519 = ADVANCED_FACE ( 'NONE', ( #1244 ), #6039, .T. ) ;
#4520 = CARTESIAN_POINT ( 'NONE',  ( 6.844556472468130259, 27.29775667647069071, -24.04598060202682319 ) ) ;
#4521 = CARTESIAN_POINT ( 'NONE',  ( 20.27158385259951956, 18.00000000000000355, 152.2284161474004520 ) ) ;
#4522 = CARTESIAN_POINT ( 'NONE',  ( -21.20617189303578343, 14.62220435867159551, 151.2938281069642130 ) ) ;
#4523 = CARTESIAN_POINT ( 'NONE',  ( 19.99999999999998579, 20.00000000000000355, 98.29316153445363113 ) ) ;
#4524 = CARTESIAN_POINT ( 'NONE',  ( 22.97500000054622760, 24.28113015263587471, 84.90069139318163138 ) ) ;
#4525 = CARTESIAN_POINT ( 'NONE',  ( 27.87500000054622262, 20.00000000000000355, 98.07665518445361386 ) ) ;
#4526 = AXIS2_PLACEMENT_3D ( 'NONE', #8998, #5132, #8804 ) ;
#4527 = CARTESIAN_POINT ( 'NONE',  ( -2.000000000000015543, 20.00000000000000355, 90.79316153445363113 ) ) ;
#4528 = CARTESIAN_POINT ( 'NONE',  ( 39.55000000109245661, 22.43689772174681707, 98.29316153445361692 ) ) ;
#4529 = EDGE_LOOP ( 'NONE', ( #10358, #4624, #6618 ) ) ;
#4530 = CARTESIAN_POINT ( 'NONE',  ( 6.000000000000000000, 4.379923479639802331, 2.528749999999992948 ) ) ;
#4531 = CARTESIAN_POINT ( 'NONE',  ( 38.65000000109246514, 20.00000000000000355, 83.29316153445364534 ) ) ;
#4532 = CARTESIAN_POINT ( 'NONE',  ( 0.000000000000000000, 22.00000000000000000, 169.9999999999999716 ) ) ;
#4533 = ORIENTED_EDGE ( 'NONE', *, *, #3245, .F. ) ;
#4534 = DIRECTION ( 'NONE',  ( 0.000000000000000000, -1.000000000000000000, 1.110768649713241713E-15 ) ) ;
#4535 = ORIENTED_EDGE ( 'NONE', *, *, #11233, .F. ) ;
#4536 = CARTESIAN_POINT ( 'NONE',  ( -1.643512924178977430, 10.13039013404520716, -24.94805769307042453 ) ) ;
#4537 = AXIS2_PLACEMENT_3D ( 'NONE', #9247, #551, #4413 ) ;
#4538 = DIRECTION ( 'NONE',  ( 0.000000000000000000, 0.000000000000000000, 1.000000000000000000 ) ) ;
#4539 = CARTESIAN_POINT ( 'NONE',  ( 29.89999999999998437, 22.43689772174679575, 98.29316153445363113 ) ) ;
#4540 = CARTESIAN_POINT ( 'NONE',  ( 12.00000000000000000, 0.000000000000000000, -6.599999999999998757 ) ) ;
#4541 = EDGE_CURVE ( 'NONE', #2307, #11430, #9937, .T. ) ;
#4542 = CARTESIAN_POINT ( 'NONE',  ( 27.89999999999998792, 22.43689772174679575, 98.29316153445363113 ) ) ;
#4543 = CARTESIAN_POINT ( 'NONE',  ( 42.69999999999998153, 13.62011893735970958, 86.15790661882942914 ) ) ;
#4544 = DIRECTION ( 'NONE',  ( 0.000000000000000000, 0.000000000000000000, -1.000000000000000000 ) ) ;
#4545 = CARTESIAN_POINT ( 'NONE',  ( 49.37500000054622973, 27.65831843345427998, 90.79316153445363113 ) ) ;
#4546 = FACE_OUTER_BOUND ( 'NONE', #8542, .T. ) ;
#4547 = AXIS2_PLACEMENT_3D ( 'NONE', #11123, #11186, #4036 ) ;
#4548 = FACE_BOUND ( 'NONE', #2128, .T. ) ;
#4549 = ORIENTED_EDGE ( 'NONE', *, *, #7622, .T. ) ;
#4550 =( BOUNDED_CURVE ( )  B_SPLINE_CURVE ( 2, ( #2631, #12281, #10362, #12093, #8349, #3334, #7199, #12215, #9242, #3517, #2506 ),
 .UNSPECIFIED., .F., .F. ) 
 B_SPLINE_CURVE_WITH_KNOTS ( ( 3, 2, 2, 2, 2, 3 ),
 ( 0.06666666666666672125, 0.07333333333333338921, 0.08000000000000007105, 0.08666666666666673902, 0.09333333333333342086, 0.1000000000000000888 ),
 .UNSPECIFIED. ) 
 CURVE ( )  GEOMETRIC_REPRESENTATION_ITEM ( )  RATIONAL_B_SPLINE_CURVE ( ( 0.9999999999999995559, 0.9510565162951539753, 1.000000000000000000, 0.9510565162951535312, 1.000000000000000000, 0.9510565162951535312, 1.000000000000000000, 0.9510565162951535312, 1.000000000000000000, 0.9510565162951529761, 1.000000000000000666 ) ) 
 REPRESENTATION_ITEM ( '' )  );
#4551 = CARTESIAN_POINT ( 'NONE',  ( 1.298299055536097368, 45.16027954822755675, 24.96835849755778014 ) ) ;
#4552 = CARTESIAN_POINT ( 'NONE',  ( 20.00000000000003908, 20.00000000000000000, 137.5000000000000000 ) ) ;
#4553 = CARTESIAN_POINT ( 'NONE',  ( 34.77500000054622831, 20.00000000000000355, 83.50966788445364841 ) ) ;
#4554 = CARTESIAN_POINT ( 'NONE',  ( 36.67500000054622689, 15.71886984736413773, 84.90069139318163138 ) ) ;
#4555 = AXIS2_PLACEMENT_3D ( 'NONE', #12039, #5252, #10136 ) ;
#4556 = CARTESIAN_POINT ( 'NONE',  ( 28.57500000054622902, 15.71886984736413773, 84.90069139318163138 ) ) ;
#4557 = EDGE_CURVE ( 'NONE', #9039, #3840, #7868, .T. ) ;
#4558 = CARTESIAN_POINT ( 'NONE',  ( 18.00000000000000355, 20.00000000000000355, 188.9999999999999716 ) ) ;
#4559 = CARTESIAN_POINT ( 'NONE',  ( 0.000000000000000000, 50.00000000000000000, -28.00000000000000711 ) ) ;
#4560 = DIRECTION ( 'NONE',  ( -0.000000000000000000, -1.000000000000000000, -0.000000000000000000 ) ) ;
#4561 = CARTESIAN_POINT ( 'NONE',  ( 31.89999999999998437, 22.43689772174679575, 98.29316153445363113 ) ) ;
#4562 = EDGE_CURVE ( 'NONE', #527, #5212, #8272, .T. ) ;
#4563 = CARTESIAN_POINT ( 'NONE',  ( 0.000000000000000000, -2.919948986426523341, 5.057500000000002771 ) ) ;
#4564 = EDGE_LOOP ( 'NONE', ( #5799, #1343 ) ) ;
#4565 = CARTESIAN_POINT ( 'NONE',  ( 34.72841614740047333, 18.00000000000000355, 152.2284161474004520 ) ) ;
#4566 = PRODUCT_CONTEXT ( 'NONE', #3909, 'mechanical' ) ;
#4567 = CARTESIAN_POINT ( 'NONE',  ( 26.17500000054622689, 13.80429023900056507, 95.29460816699764791 ) ) ;
#4568 = CARTESIAN_POINT ( 'NONE',  ( 26.65000000109246514, 20.00000000000000355, 83.29316153445364534 ) ) ;
#4569 = VECTOR ( 'NONE', #7668, 1000.000000000000000 ) ;
#4570 = CARTESIAN_POINT ( 'NONE',  ( 48.37500000054622973, 13.07298590277314432, 88.54243821818161564 ) ) ;
#4571 = CARTESIAN_POINT ( 'NONE',  ( 32.67500000054622689, 15.71886984736413773, 84.90069139318163138 ) ) ;
#4572 = CARTESIAN_POINT ( 'NONE',  ( 28.89999999999998437, 17.56310227825321135, 83.29316153445363113 ) ) ;
#4573 = CIRCLE ( 'NONE', #3753, 28.00000000000000355 ) ;
#4574 = CARTESIAN_POINT ( 'NONE',  ( 9.465308527890080370, 23.24274166418333110, 23.13911695433847981 ) ) ;
#4575 = CARTESIAN_POINT ( 'NONE',  ( 36.67500000054623399, 17.63344945572770328, 83.50966788445364841 ) ) ;
#4576 = VERTEX_POINT ( 'NONE', #8787 ) ;
#4577 = ADVANCED_FACE ( 'NONE', ( #105 ), #7901, .T. ) ;
#4578 = CARTESIAN_POINT ( 'NONE',  ( 20.55000000109246372, 17.56310227825321135, 83.29316153445363113 ) ) ;
#4579 = LINE ( 'NONE', #10283, #2244 ) ;
#4580 = ORIENTED_EDGE ( 'NONE', *, *, #6365, .F. ) ;
#4581 = CARTESIAN_POINT ( 'NONE',  ( -8.486922698271502696, 25.29893941662590251, -26.68348577013889056 ) ) ;
#4582 = VERTEX_POINT ( 'NONE', #9811 ) ;
#4583 =( LENGTH_UNIT ( ) NAMED_UNIT ( * ) SI_UNIT ( .MILLI., .METRE. ) );
#4584 = CARTESIAN_POINT ( 'NONE',  ( -50.00000000000001421, 22.00000000000000000, 152.2284161474004520 ) ) ;
#4585 = EDGE_CURVE ( 'NONE', #11119, #10746, #6848, .T. ) ;
#4586 = CARTESIAN_POINT ( 'NONE',  ( 0.3265943374146230704, 45.00000000000000711, -28.00000000000000000 ) ) ;
#4587 = DIRECTION ( 'NONE',  ( 0.000000000000000000, -1.000000000000000000, 0.000000000000000000 ) ) ;
#4588 = CARTESIAN_POINT ( 'NONE',  ( 26.07500000054622902, 13.80429023900056507, 95.29460816699764791 ) ) ;
#4589 = CARTESIAN_POINT ( 'NONE',  ( 21.67500000054622333, 24.28113015263587116, 96.68563167572563088 ) ) ;
#4590 = CIRCLE ( 'NONE', #6213, 8.400000000000000355 ) ;
#4591 = CARTESIAN_POINT ( 'NONE',  ( -2.290944097510326571, 29.73958545346254922, -24.89690719708686828 ) ) ;
#4592 = EDGE_CURVE ( 'NONE', #5728, #10127, #8847, .T. ) ;
#4593 = CARTESIAN_POINT ( 'NONE',  ( -3.768871583585197360, 46.69794849765531808, 24.71539284385418611 ) ) ;
#4594 = ORIENTED_EDGE ( 'NONE', *, *, #7758, .F. ) ;
#4595 = CARTESIAN_POINT ( 'NONE',  ( 39.85000000109246798, 15.59161060780645691, 96.86078899226572503 ) ) ;
#4596 = CARTESIAN_POINT ( 'NONE',  ( 23.99999999999998579, 20.00000000000000355, 98.29316153445363113 ) ) ;
#4597 = ORIENTED_EDGE ( 'NONE', *, *, #9414, .F. ) ;
#4598 = PRESENTATION_STYLE_ASSIGNMENT (( #6979 ) ) ;
#4599 = ORIENTED_EDGE ( 'NONE', *, *, #1038, .F. ) ;
#4600 = CARTESIAN_POINT ( 'NONE',  ( -0.6576044892141179599, 10.01619439626406383, -24.99350884773162207 ) ) ;
#4601 = CIRCLE ( 'NONE', #12299, 6.999999999999978684 ) ;
#4602 = DIRECTION ( 'NONE',  ( 0.000000000000000000, 0.4999999999999987232, -0.8660254037844393737 ) ) ;
#4603 = CARTESIAN_POINT ( 'NONE',  ( -2.000000000000015543, 20.00000000000000355, 98.29316153445363113 ) ) ;
#4604 = DIRECTION ( 'NONE',  ( 0.000000000000000000, 0.000000000000000000, -1.000000000000000000 ) ) ;
#4605 = CARTESIAN_POINT ( 'NONE',  ( -1.614219986190975620, 45.25635288715552207, 20.94008338602824182 ) ) ;
#4606 = CARTESIAN_POINT ( 'NONE',  ( -6.999999999999999112, 92.00000000000000000, 69.99999999999998579 ) ) ;
#4607 = CARTESIAN_POINT ( 'NONE',  ( 48.57500000054622546, 13.80429023900056684, 86.29171490190961435 ) ) ;
#4608 = AXIS2_PLACEMENT_3D ( 'NONE', #2569, #4356, #12159 ) ;
#4609 = CARTESIAN_POINT ( 'NONE',  ( 9.737811142203947057, 22.29842083447240597, 23.02563804066124931 ) ) ;
#4610 = DIRECTION ( 'NONE',  ( 0.000000000000000000, 0.000000000000000000, 1.000000000000000000 ) ) ;
#4611 = ORIENTED_EDGE ( 'NONE', *, *, #100, .T. ) ;
#4612 = EDGE_LOOP ( 'NONE', ( #2688, #6512 ) ) ;
#4613 = CARTESIAN_POINT ( 'NONE',  ( 43.45000000109246230, 24.40838939219354842, 96.86078899226572503 ) ) ;
#4614 = DIRECTION ( 'NONE',  ( -0.000000000000000000, -1.000000000000000000, -0.000000000000000000 ) ) ;
#4615 = CARTESIAN_POINT ( 'NONE',  ( 37.47500000054622404, 26.92701409722686634, 93.04388485072563242 ) ) ;
#4616 = CARTESIAN_POINT ( 'NONE',  ( 20.07500000054622546, 13.80429023900056507, 95.29460816699764791 ) ) ;
#4617 = CARTESIAN_POINT ( 'NONE',  ( 49.99999999999998579, 40.00000000000000000, 69.99999999999998579 ) ) ;
#4618 = CARTESIAN_POINT ( 'NONE',  ( -50.00000000000001421, 69.50000000000000000, 146.8533255156881978 ) ) ;
#4619 = CARTESIAN_POINT ( 'NONE',  ( -2.508870892452910173, 54.33730018467829126, -20.85139144392807253 ) ) ;
#4620 = LINE ( 'NONE', #6641, #10796 ) ;
#4621 =( BOUNDED_CURVE ( )  B_SPLINE_CURVE ( 2, ( #6121, #9990, #412, #1302, #5173, #4218, #8090, #11956, #2311, #6180, #4275 ),
 .UNSPECIFIED., .F., .F. ) 
 B_SPLINE_CURVE_WITH_KNOTS ( ( 3, 2, 2, 2, 2, 3 ),
 ( 0.2666666666666666630, 0.2733333333333333171, 0.2800000000000000266, 0.2866666666666666807, 0.2933333333333333348, 0.2999999999999999889 ),
 .UNSPECIFIED. ) 
 CURVE ( )  GEOMETRIC_REPRESENTATION_ITEM ( )  RATIONAL_B_SPLINE_CURVE ( ( 1.000000000000000000, 0.9510565162951535312, 1.000000000000000000, 0.9510565162951535312, 1.000000000000000000, 0.9510565162951535312, 1.000000000000000000, 0.9510565162951535312, 1.000000000000000000, 0.9510565162951535312, 1.000000000000000000 ) ) 
 REPRESENTATION_ITEM ( '' )  );
#4622 = AXIS2_PLACEMENT_3D ( 'NONE', #1557, #540, #4347 ) ;
#4623 = DIRECTION ( 'NONE',  ( -1.000000000000000000, -0.000000000000000000, -0.000000000000000000 ) ) ;
#4624 = ORIENTED_EDGE ( 'NONE', *, *, #11327, .T. ) ;
#4625 = DIRECTION ( 'NONE',  ( 0.000000000000000000, 0.000000000000000000, -1.000000000000000000 ) ) ;
#4626 = EDGE_CURVE ( 'NONE', #8571, #8548, #2917, .T. ) ;
#4627 = CARTESIAN_POINT ( 'NONE',  ( -7.589415207398531038E-16, 49.99999999999999289, -46.16807740719850273 ) ) ;
#4628 = B_SPLINE_CURVE_WITH_KNOTS ( 'NONE', 3,
 ( #5512, #10438, #8483, #622, #2581, #9320, #7278, #3593, #4486, #11149, #5630, #12108, #9379, #10256, #4421, #558, #8361, #5447, #12354, #12292 ),
 .UNSPECIFIED., .F., .F.,
 ( 4, 2, 2, 2, 2, 2, 2, 2, 2, 4 ),
 ( 0.01567180661725443153, 0.01665134708417310289, 0.01763088755109177425, 0.01812065778455110993, 0.01861042801801044561, 0.01958996848492911697, 0.02056950895184778833, 0.02154904941876645622, 0.02252858988568512758, 0.02350813035260379893 ),
 .UNSPECIFIED. ) ;
#4629 = VECTOR ( 'NONE', #2333, 1000.000000000000000 ) ;
#4630 = CARTESIAN_POINT ( 'NONE',  ( 27.97500000054622404, 17.63344945572769973, 98.07665518445361386 ) ) ;
#4631 = CARTESIAN_POINT ( 'NONE',  ( 89.17200000000001125, 0.000000000000000000, 0.000000000000000000 ) ) ;
#4632 = CARTESIAN_POINT ( 'NONE',  ( 37.67500000054622689, 22.36655054427230027, 98.07665518445361386 ) ) ;
#4633 = CARTESIAN_POINT ( 'NONE',  ( 28.57500000054622191, 13.80429023900056684, 86.29171490190961435 ) ) ;
#4634 = CARTESIAN_POINT ( 'NONE',  ( 28.29999999999998650, 13.62011893735971135, 95.42841645007781892 ) ) ;
#4635 = CARTESIAN_POINT ( 'NONE',  ( 40.47500000054622404, 13.80429023900056684, 86.29171490190961435 ) ) ;
#4636 = ORIENTED_EDGE ( 'NONE', *, *, #6111, .T. ) ;
#4637 = CARTESIAN_POINT ( 'NONE',  ( 20.25000000109246301, 12.86707612778636012, 88.47553407664152303 ) ) ;
#4638 = CARTESIAN_POINT ( 'NONE',  ( -3.302322679538425287, 46.23143709543641933, -20.74005723812733848 ) ) ;
#4639 = ORIENTED_EDGE ( 'NONE', *, *, #6839, .T. ) ;
#4640 = VECTOR ( 'NONE', #10947, 1000.000000000000000 ) ;
#4641 = CARTESIAN_POINT ( 'NONE',  ( 7.297852186526522900, 13.15569421923598448, 19.69262651265845676 ) ) ;
#4642 = ORIENTED_EDGE ( 'NONE', *, *, #8971, .F. ) ;
#4643 = VECTOR ( 'NONE', #7266, 1000.000000000000000 ) ;
#4644 = DIRECTION ( 'NONE',  ( 1.000000000000000000, -0.000000000000000000, -0.000000000000000000 ) ) ;
#4645 = CYLINDRICAL_SURFACE ( 'NONE', #1805, 7.499999999999992895 ) ;
#4646 = CARTESIAN_POINT ( 'NONE',  ( 3.061616997868383043E-15, 0.000000000000000000, 25.00000000000000000 ) ) ;
#4647 = CARTESIAN_POINT ( 'NONE',  ( 42.37500000054621552, 12.34168156654572357, 90.79316153445363113 ) ) ;
#4648 = DIRECTION ( 'NONE',  ( -1.000000000000000000, -0.000000000000000000, -0.000000000000000000 ) ) ;
#4649 = ADVANCED_FACE ( 'NONE', ( #6129 ), #3329, .F. ) ;
#4650 = CARTESIAN_POINT ( 'NONE',  ( 43.57500000054623257, 26.19570976099943493, 95.29460816699764791 ) ) ;
#4651 = CARTESIAN_POINT ( 'NONE',  ( 47.29999999999998295, 26.37988106264029398, 86.15790661882942914 ) ) ;
#4652 = B_SPLINE_CURVE_WITH_KNOTS ( 'NONE', 3,
 ( #769, #1776, #7624, #5660, #5723, #7498, #8509, #8573, #7370, #4638, #9408, #12259, #12384, #1600, #10465, #10406, #11487, #2675 ),
 .UNSPECIFIED., .F., .F.,
 ( 4, 2, 2, 2, 2, 2, 2, 2, 4 ),
 ( 0.007846449623959500519, 0.008826741871943226750, 0.009807034119926952981, 0.01078732636791067921, 0.01176761861589440544, 0.01274791086387813341, 0.01372820311186185790, 0.01470849535984558587, 0.01568878760782931384 ),
 .UNSPECIFIED. ) ;
#4653 = LINE ( 'NONE', #10419, #4344 ) ;
#4654 = CARTESIAN_POINT ( 'NONE',  ( -2.645619823791141467, 45.75416279094086036, 24.85999165416970413 ) ) ;
#4655 = EDGE_LOOP ( 'NONE', ( #5702, #9321, #4699, #2094 ) ) ;
#4656 = CARTESIAN_POINT ( 'NONE',  ( 36.55000000109247082, 17.56310227825321135, 83.29316153445363113 ) ) ;
#4657 = CARTESIAN_POINT ( 'NONE',  ( 24.19999999999998863, 15.59161060780645691, 96.86078899226572503 ) ) ;
#4658 = EDGE_LOOP ( 'NONE', ( #12076, #996, #1245, #12536 ) ) ;
#4659 = FILL_AREA_STYLE ('',( #728 ) ) ;
#4660 = VERTEX_POINT ( 'NONE', #9173 ) ;
#4661 = TOROIDAL_SURFACE ( 'NONE', #9531, 17.50000000000000355, 10.00000000000000000 ) ;
#4662 = CARTESIAN_POINT ( 'NONE',  ( 10.00000000000000355, 20.00000000000000355, -70.00000000000000000 ) ) ;
#4663 = CARTESIAN_POINT ( 'NONE',  ( 30.65000000109246514, 20.00000000000000355, 83.29316153445364534 ) ) ;
#4664 = B_SPLINE_CURVE_WITH_KNOTS ( 'NONE', 3,
 ( #1493, #12028, #3332, #5370, #9240, #9302, #543, #8284, #7324, #7387, #4468, #7514, #7451, #6615, #8467, #6679, #1736, #3827, #5681, #2815 ),
 .UNSPECIFIED., .F., .F.,
 ( 4, 2, 2, 2, 2, 2, 2, 2, 2, 4 ),
 ( 0.02350824016915415912, 0.02448716854195917558, 0.02546609691476419204, 0.02644502528756920851, 0.02693448947397171500, 0.02742395366037422497, 0.02840288203317925531, 0.02938181040598428218, 0.03036073877878931251, 0.03133966715159434285 ),
 .UNSPECIFIED. ) ;
#4665 = EDGE_CURVE ( 'NONE', #11427, #10229, #7194, .T. ) ;
#4666 = CARTESIAN_POINT ( 'NONE',  ( -9.918452521082530282, 21.31677563331469116, 22.94832388515032662 ) ) ;
#4667 = FACE_OUTER_BOUND ( 'NONE', #4529, .T. ) ;
#4668 = LINE ( 'NONE', #3839, #11127 ) ;
#4669 = VERTEX_POINT ( 'NONE', #11071 ) ;
#4670 = CIRCLE ( 'NONE', #1442, 5.035999999999999588 ) ;
#4671 = CARTESIAN_POINT ( 'NONE',  ( -50.00000000000001421, 40.00000000000000000, 69.99999999999998579 ) ) ;
#4672 = EDGE_CURVE ( 'NONE', #1996, #58, #4224, .T. ) ;
#4673 = CARTESIAN_POINT ( 'NONE',  ( -3.237458362839043868, 10.51577337999971640, 27.81894738099048325 ) ) ;
#4674 = CARTESIAN_POINT ( 'NONE',  ( 47.37500000054622973, 27.65831843345427998, 90.79316153445363113 ) ) ;
#4675 = CARTESIAN_POINT ( 'NONE',  ( -2.000000000000015543, 20.00000000000000355, 98.29316153445363113 ) ) ;
#4676 = DIRECTION ( 'NONE',  ( 0.000000000000000000, -0.4999999999999989453, 0.8660254037844393737 ) ) ;
#4677 = ORIENTED_EDGE ( 'NONE', *, *, #6421, .F. ) ;
#4678 = ORIENTED_EDGE ( 'NONE', *, *, #3662, .F. ) ;
#4679 = EDGE_CURVE ( 'NONE', #1426, #11906, #11193, .T. ) ;
#4680 = AXIS2_PLACEMENT_3D ( 'NONE', #1662, #714, #12321 ) ;
#4681 = CARTESIAN_POINT ( 'NONE',  ( -3.567510909640027705, 29.34773727012557387, -20.69703671296004188 ) ) ;
#4682 = LINE ( 'NONE', #5575, #5620 ) ;
#4683 = CARTESIAN_POINT ( 'NONE',  ( 20.37500000054622618, 13.07298590277314432, 88.54243821818161564 ) ) ;
#4684 = CARTESIAN_POINT ( 'NONE',  ( 4.999999999999999112, 40.00000000000000000, 169.9999999999999716 ) ) ;
#4685 = CARTESIAN_POINT ( 'NONE',  ( -2.222058947943490903, 54.49108331096404356, -20.88431890158240734 ) ) ;
#4686 = FACE_OUTER_BOUND ( 'NONE', #7090, .T. ) ;
#4687 = LINE ( 'NONE', #8558, #4569 ) ;
#4688 = CARTESIAN_POINT ( 'NONE',  ( -10.00000000000000355, 20.00000000000000355, -66.99999999999998579 ) ) ;
#4689 = ORIENTED_EDGE ( 'NONE', *, *, #5994, .F. ) ;
#4690 = CYLINDRICAL_SURFACE ( 'NONE', #8536, 7.500000000000000000 ) ;
#4691 =( LENGTH_UNIT ( ) NAMED_UNIT ( * ) SI_UNIT ( .MILLI., .METRE. ) );
#4692 = CARTESIAN_POINT ( 'NONE',  ( 36.19999999999998863, 15.59161060780645691, 96.86078899226572503 ) ) ;
#4693 = CARTESIAN_POINT ( 'NONE',  ( 36.67500000054622689, 17.63344945572770328, 83.50966788445364841 ) ) ;
#4694 = CARTESIAN_POINT ( 'NONE',  ( 30.87500000054622618, 20.00000000000000355, 83.50966788445364841 ) ) ;
#4695 = CARTESIAN_POINT ( 'NONE',  ( 30.49999999999998934, 12.11403331821300533, 90.79316153445363113 ) ) ;
#4696 = CARTESIAN_POINT ( 'NONE',  ( 30.89999999999998437, 17.56310227825320425, 83.29316153445363113 ) ) ;
#4697 = EDGE_CURVE ( 'NONE', #3463, #5153, #11962, .T. ) ;
#4698 = CARTESIAN_POINT ( 'NONE',  ( 39.77500000054622831, 20.00000000000000355, 98.07665518445361386 ) ) ;
#4699 = ORIENTED_EDGE ( 'NONE', *, *, #4079, .T. ) ;
#4700 = CARTESIAN_POINT ( 'NONE',  ( 20.15000000109246514, 12.11403331821300533, 90.79316153445363113 ) ) ;
#4701 = CYLINDRICAL_SURFACE ( 'NONE', #12165, 8.000000000000000000 ) ;
#4702 = ORIENTED_EDGE ( 'NONE', *, *, #2513, .T. ) ;
#4703 = CARTESIAN_POINT ( 'NONE',  ( -4.452344947754465210, 28.97817800798833332, -27.65051488940038737 ) ) ;
#4704 = VERTEX_POINT ( 'NONE', #2261 ) ;
#4705 = CARTESIAN_POINT ( 'NONE',  ( 9.355409448593292154, 23.54720254436722371, -23.18392859692124830 ) ) ;
#4706 = DIRECTION ( 'NONE',  ( 0.000000000000000000, 0.000000000000000000, 1.000000000000000000 ) ) ;
#4707 = FACE_OUTER_BOUND ( 'NONE', #3904, .T. ) ;
#4708 = CARTESIAN_POINT ( 'NONE',  ( 41.97500000054623115, 17.63344945572769973, 98.07665518445361386 ) ) ;
#4709 = CARTESIAN_POINT ( 'NONE',  ( 20.69999999999998508, 13.62011893735970958, 86.15790661882942914 ) ) ;
#4710 = DIRECTION ( 'NONE',  ( 0.000000000000000000, -1.000000000000000000, -0.000000000000000000 ) ) ;
#4711 = CARTESIAN_POINT ( 'NONE',  ( 42.97500000054622404, 22.36655054427230382, 83.50966788445364841 ) ) ;
#4712 = CARTESIAN_POINT ( 'NONE',  ( 20.57500000054622546, 13.80429023900056684, 86.29171490190961435 ) ) ;
#4713 = CARTESIAN_POINT ( 'NONE',  ( 6.000000000000000000, -2.919948986426523341, 5.057500000000002771 ) ) ;
#4714 = CYLINDRICAL_SURFACE ( 'NONE', #2194, 10.00000000000000355 ) ;
#4715 = ORIENTED_EDGE ( 'NONE', *, *, #8147, .F. ) ;
#4716 = AXIS2_PLACEMENT_3D ( 'NONE', #10989, #11172, #9153 ) ;
#4717 = CARTESIAN_POINT ( 'NONE',  ( 34.55000000109247082, 17.56310227825321135, 83.29316153445363113 ) ) ;
#4718 =( LENGTH_UNIT ( ) NAMED_UNIT ( * ) SI_UNIT ( .MILLI., .METRE. ) );
#4719 = ORIENTED_EDGE ( 'NONE', *, *, #1424, .T. ) ;
#4720 = DIRECTION ( 'NONE',  ( 0.000000000000000000, 0.000000000000000000, 1.000000000000000000 ) ) ;
#4721 = ADVANCED_FACE ( 'NONE', ( #4280 ), #2438, .T. ) ;
#4722 = ORIENTED_EDGE ( 'NONE', *, *, #6731, .T. ) ;
#4723 = DIRECTION ( 'NONE',  ( -0.000000000000000000, -0.000000000000000000, 1.000000000000000000 ) ) ;
#4724 = CARTESIAN_POINT ( 'NONE',  ( 20.27158385259951956, 22.00000000000000000, 169.9999999999999716 ) ) ;
#4725 = LINE ( 'NONE', #733, #7784 ) ;
#4726 = EDGE_CURVE ( 'NONE', #8716, #9224, #5304, .T. ) ;
#4727 = CIRCLE ( 'NONE', #12228, 25.00000000000000000 ) ;
#4728 = LINE ( 'NONE', #8477, #10427 ) ;
#4729 = PLANE ( 'NONE',  #11330 ) ;
#4730 = ORIENTED_EDGE ( 'NONE', *, *, #8073, .T. ) ;
#4731 = DIRECTION ( 'NONE',  ( 0.000000000000000000, -0.5000000000000011102, -0.8660254037844380415 ) ) ;
#4732 = DIRECTION ( 'NONE',  ( 0.000000000000000000, 0.000000000000000000, 1.000000000000000000 ) ) ;
#4733 = CARTESIAN_POINT ( 'NONE',  ( 48.77500000054623541, 17.63344945572770328, 83.50966788445364841 ) ) ;
#4734 = ORIENTED_EDGE ( 'NONE', *, *, #3098, .F. ) ;
#4735 = CARTESIAN_POINT ( 'NONE',  ( 45.75000000109247367, 17.56310227825317227, 98.29316153445361692 ) ) ;
#4736 = VECTOR ( 'NONE', #10741, 1000.000000000000000 ) ;
#4737 = CARTESIAN_POINT ( 'NONE',  ( -5.000000000000002665, 18.00000000000000355, 152.2284161474004520 ) ) ;
#4738 = VERTEX_POINT ( 'NONE', #10183 ) ;
#4739 = ORIENTED_EDGE ( 'NONE', *, *, #2258, .T. ) ;
#4740 = PRODUCT_DEFINITION_FORMATION_WITH_SPECIFIED_SOURCE ( 'ANY', '', #5086, .NOT_KNOWN. ) ;
#4741 = B_SPLINE_CURVE_WITH_KNOTS ( 'NONE', 3,
 ( #5562, #924, #855, #7647, #1740, #11510, #10611, #2697, #7521, #7456, #8473, #11451, #794, #9371, #8657, #9555, #8594, #2821, #12526, #7709, #11577, #2884, #2636, #5502, #671, #6501, #1679, #9431 ),
 .UNSPECIFIED., .F., .F.,
 ( 4, 2, 2, 2, 2, 2, 2, 2, 2, 2, 2, 2, 2, 4 ),
 ( 0.03175360674246840986, 0.03274498614013845316, 0.03373636553780849645, 0.03571912433314858998, 0.03671050373081863327, 0.03770188312848867657, 0.03869326252615871986, 0.03968464192382877009, 0.04166740071916885668, 0.04265878011683889998, 0.04365015951450894327, 0.04563291830984904374, 0.04662429770751908703, 0.04761567710518913032 ),
 .UNSPECIFIED. ) ;
#4742 = CARTESIAN_POINT ( 'NONE',  ( -2.301101458689752910, 29.73723473350772650, -20.87607290278878835 ) ) ;
#4743 = EDGE_CURVE ( 'NONE', #10068, #9549, #1490, .T. ) ;
#4744 = CARTESIAN_POINT ( 'NONE',  ( 6.000000000000000000, 0.000000000000000000, 0.000000000000000000 ) ) ;
#4745 = CARTESIAN_POINT ( 'NONE',  ( 22.17500000054622689, 13.07298590277314254, 93.04388485072563242 ) ) ;
#4746 = DIRECTION ( 'NONE',  ( 0.000000000000000000, 1.000000000000000000, -1.224646799147353207E-16 ) ) ;
#4747 = AXIS2_PLACEMENT_3D ( 'NONE', #12024, #7193, #5736 ) ;
#4748 = CARTESIAN_POINT ( 'NONE',  ( -3.766953629715470431, 53.30388651120591703, -20.66069581306526004 ) ) ;
#4749 = CARTESIAN_POINT ( 'NONE',  ( 3.024050948510435495E-21, 45.00000000000000711, -21.00000000000000000 ) ) ;
#4750 = EDGE_CURVE ( 'NONE', #10247, #12336, #11903, .T. ) ;
#4751 = CARTESIAN_POINT ( 'NONE',  ( 25.75000000109246301, 17.56310227825320425, 98.29316153445363113 ) ) ;
#4752 = LINE ( 'NONE', #1889, #8327 ) ;
#4753 = ORIENTED_EDGE ( 'NONE', *, *, #12049, .T. ) ;
#4754 = CARTESIAN_POINT ( 'NONE',  ( 6.000000000000000000, 2.919948986426538884, 5.057499999999996554 ) ) ;
#4755 = DIRECTION ( 'NONE',  ( 0.000000000000000000, 0.000000000000000000, -1.000000000000000000 ) ) ;
#4756 = AXIS2_PLACEMENT_3D ( 'NONE', #12104, #6326, #6264 ) ;
#4757 = CARTESIAN_POINT ( 'NONE',  ( 27.87500000054622262, 20.00000000000000355, 98.07665518445361386 ) ) ;
#4758 = CARTESIAN_POINT ( 'NONE',  ( 121.0360000000000156, 0.000000000000000000, 0.000000000000000000 ) ) ;
#4759 = CARTESIAN_POINT ( 'NONE',  ( 41.87500000054621552, 17.63344945572769973, 98.07665518445361386 ) ) ;
#4760 = CARTESIAN_POINT ( 'NONE',  ( 26.87500000054622618, 20.00000000000000355, 83.50966788445364841 ) ) ;
#4761 = CARTESIAN_POINT ( 'NONE',  ( 31.09999999999999076, 22.43689772174679575, 83.29316153445363113 ) ) ;
#4762 = B_SPLINE_CURVE_WITH_KNOTS ( 'NONE', 3,
 ( #6954, #4100, #8863, #9948, #9759, #1256, #1068, #7979, #3400, #6261, #8231, #11976, #3220, #11081, #2270, #5251, #4235, #9312, #2514, #7271 ),
 .UNSPECIFIED., .F., .F.,
 ( 4, 2, 2, 2, 2, 2, 2, 2, 2, 4 ),
 ( 0.02350813035260379893, 0.02448705762280033518, 0.02546598489299686796, 0.02644491216319340421, 0.02693437579829167233, 0.02742383943338994046, 0.02840276670358647670, 0.02938169397378300948, 0.03036062124397954226, 0.03133954851417607851 ),
 .UNSPECIFIED. ) ;
#4763 = DIRECTION ( 'NONE',  ( 1.000000000000000000, 0.000000000000000000, 0.000000000000000000 ) ) ;
#4764 = CARTESIAN_POINT ( 'NONE',  ( 33.57500000054623257, 24.28113015263587116, 96.68563167572563088 ) ) ;
#4765 = ORIENTED_EDGE ( 'NONE', *, *, #10552, .F. ) ;
#4766 = CIRCLE ( 'NONE', #3146, 5.057500000000000107 ) ;
#4767 = CARTESIAN_POINT ( 'NONE',  ( 41.97500000054623115, 15.71886984736413417, 96.68563167572563088 ) ) ;
#4768 = DIRECTION ( 'NONE',  ( 0.000000000000000000, 0.000000000000000000, 1.000000000000000000 ) ) ;
#4769 = ORIENTED_EDGE ( 'NONE', *, *, #9171, .T. ) ;
#4770 = CARTESIAN_POINT ( 'NONE',  ( 3.245314017740486554E-15, -3.000000000000003109, -25.00000000000000355 ) ) ;
#4771 = ORIENTED_EDGE ( 'NONE', *, *, #11626, .F. ) ;
#4772 = CARTESIAN_POINT ( 'NONE',  ( 1.651856453710261352, 29.86806670974593914, -24.94744891504881679 ) ) ;
#4773 = CARTESIAN_POINT ( 'NONE',  ( 32.39999999999998437, 12.86707612778636012, 93.11078899226572503 ) ) ;
#4774 = CIRCLE ( 'NONE', #7816, 9.000000000000000000 ) ;
#4775 = DIRECTION ( 'NONE',  ( -0.000000000000000000, 0.000000000000000000, 1.000000000000000000 ) ) ;
#4776 = CARTESIAN_POINT ( 'NONE',  ( 45.27500000054622831, 26.92701409722686634, 88.54243821818162985 ) ) ;
#4777 = DIRECTION ( 'NONE',  ( -1.000000000000000000, -0.000000000000000000, -0.000000000000000000 ) ) ;
#4778 =( NAMED_UNIT ( * ) PLANE_ANGLE_UNIT ( ) SI_UNIT ( $, .RADIAN. ) );
#4779 = CARTESIAN_POINT ( 'NONE',  ( 45.37500000054622973, 27.65831843345427998, 90.79316153445363113 ) ) ;
#4780 = CARTESIAN_POINT ( 'NONE',  ( 20.67500000054622689, 15.71886984736413773, 84.90069139318163138 ) ) ;
#4781 = CARTESIAN_POINT ( 'NONE',  ( 0.000000000000000000, -2.919948986426538440, -5.057499999999997442 ) ) ;
#4782 = CARTESIAN_POINT ( 'NONE',  ( 49.57500000054623257, 24.28113015263587116, 96.68563167572563088 ) ) ;
#4783 = ORIENTED_EDGE ( 'NONE', *, *, #12173, .F. ) ;
#4784 = CARTESIAN_POINT ( 'NONE',  ( 37.35000000109246088, 26.37988106264029398, 95.42841645007781892 ) ) ;
#4785 = CARTESIAN_POINT ( 'NONE',  ( 23.99999999999998579, 20.00000000000000355, 98.29316153445363113 ) ) ;
#4786 = ORIENTED_EDGE ( 'NONE', *, *, #764, .F. ) ;
#4787 = FACE_OUTER_BOUND ( 'NONE', #8725, .T. ) ;
#4788 = ORIENTED_EDGE ( 'NONE', *, *, #11212, .T. ) ;
#4789 = DIRECTION ( 'NONE',  ( 0.000000000000000000, 1.000000000000000000, 0.000000000000000000 ) ) ;
#4790 = CARTESIAN_POINT ( 'NONE',  ( 31.55000000109246727, 22.43689772174679575, 98.29316153445363113 ) ) ;
#4791 = EDGE_CURVE ( 'NONE', #4846, #8548, #480, .T. ) ;
#4792 = CARTESIAN_POINT ( 'NONE',  ( -2.000000000000015543, 20.00000000000000355, 98.29316153445363113 ) ) ;
#4793 = AXIS2_PLACEMENT_3D ( 'NONE', #3152, #10893, #6079 ) ;
#4794 = CARTESIAN_POINT ( 'NONE',  ( 36.17500000054622689, 13.07298590277314254, 93.04388485072563242 ) ) ;
#4795 = CARTESIAN_POINT ( 'NONE',  ( 5.000000000000000000, 4.685197434473814759, -5.637851296924623057E-15 ) ) ;
#4796 = CARTESIAN_POINT ( 'NONE',  ( 27.09999999999998721, 22.43689772174683128, 83.29316153445365956 ) ) ;
#4797 = VERTEX_POINT ( 'NONE', #8157 ) ;
#4798 = DIRECTION ( 'NONE',  ( -1.000000000000000000, -0.000000000000000000, -0.000000000000000000 ) ) ;
#4799 = CARTESIAN_POINT ( 'NONE',  ( 48.45000000109246940, 15.59161060780646046, 84.72553407664153724 ) ) ;
#4800 = CARTESIAN_POINT ( 'NONE',  ( 49.47500000054623115, 26.92701409722686634, 93.04388485072563242 ) ) ;
#4801 = ORIENTED_EDGE ( 'NONE', *, *, #6893, .F. ) ;
#4802 = CARTESIAN_POINT ( 'NONE',  ( 1.500000000000001332, 0.000000000000000000, 6.500000000000000888 ) ) ;
#4803 = UNCERTAINTY_MEASURE_WITH_UNIT (LENGTH_MEASURE( 1.000000000000000082E-05 ), #4718, 'distance_accuracy_value', 'NONE');
#4804 = CARTESIAN_POINT ( 'NONE',  ( -2.000000000000015543, 20.00000000000000355, 90.79316153445363113 ) ) ;
#4805 = EDGE_LOOP ( 'NONE', ( #11057, #1481, #1658, #1558, #2002 ) ) ;
#4806 = CIRCLE ( 'NONE', #8050, 7.500000000000000000 ) ;
#4807 = VERTEX_POINT ( 'NONE', #8280 ) ;
#4808 = CARTESIAN_POINT ( 'NONE',  ( 21.89999999999998437, 22.43689772174679575, 98.29316153445363113 ) ) ;
#4809 = CARTESIAN_POINT ( 'NONE',  ( 0.6000000000000033085, 0.000000000000000000, 0.000000000000000000 ) ) ;
#4810 = EDGE_CURVE ( 'NONE', #3699, #1672, #5643, .T. ) ;
#4811 = EDGE_CURVE ( 'NONE', #6575, #11047, #5390, .T. ) ;
#4812 = VECTOR ( 'NONE', #11931, 1000.000000000000000 ) ;
#4813 = CARTESIAN_POINT ( 'NONE',  ( 20.87500000054622618, 22.36655054427230382, 83.50966788445364841 ) ) ;
#4814 = DIRECTION ( 'NONE',  ( 0.000000000000000000, -0.4999999999999989453, 0.8660254037844393737 ) ) ;
#4815 = DIRECTION ( 'NONE',  ( 1.000000000000000000, 0.000000000000000000, 0.000000000000000000 ) ) ;
#4816 = CARTESIAN_POINT ( 'NONE',  ( 25.65000000109246514, 20.00000000000000355, 98.29316153445363113 ) ) ;
#4817 = DIRECTION ( 'NONE',  ( 0.000000000000000000, -0.5000000000000011102, -0.8660254037844380415 ) ) ;
#4818 = VERTEX_POINT ( 'NONE', #6676 ) ;
#4819 = CARTESIAN_POINT ( 'NONE',  ( 10.00000000000000711, 20.65896320323604485, -22.91287847477919470 ) ) ;
#4820 = CONICAL_SURFACE ( 'NONE', #6439, 26.49999999999999645, 0.7853981633974517207 ) ;
#4821 = APPLICATION_PROTOCOL_DEFINITION ( 'draft international standard', 'automotive_design', 1998, #8218 ) ;
#4822 =( BOUNDED_CURVE ( )  B_SPLINE_CURVE ( 2, ( #913, #8403, #2559, #1790, #1854, #7573, #12273, #12455, #11441, #5677, #7510 ),
 .UNSPECIFIED., .F., .F. ) 
 B_SPLINE_CURVE_WITH_KNOTS ( ( 3, 2, 2, 2, 2, 3 ),
 ( 0.2666666666666666630, 0.2733333333333333171, 0.2800000000000000266, 0.2866666666666666807, 0.2933333333333333348, 0.2999999999999999889 ),
 .UNSPECIFIED. ) 
 CURVE ( )  GEOMETRIC_REPRESENTATION_ITEM ( )  RATIONAL_B_SPLINE_CURVE ( ( 1.000000000000000000, 0.9510565162951535312, 1.000000000000000000, 0.9510565162951535312, 1.000000000000000000, 0.9510565162951535312, 1.000000000000000000, 0.9510565162951535312, 1.000000000000000000, 0.9510565162951535312, 1.000000000000000000 ) ) 
 REPRESENTATION_ITEM ( '' )  );
#4823 = EDGE_CURVE ( 'NONE', #5090, #9971, #12395, .T. ) ;
#4824 = CARTESIAN_POINT ( 'NONE',  ( 0.000000000000000000, 5.839897972853064445, -8.673617379884035472E-15 ) ) ;
#4825 = CARTESIAN_POINT ( 'NONE',  ( 41.27500000054622831, 27.65831843345427998, 90.79316153445363113 ) ) ;
#4826 = AXIS2_PLACEMENT_3D ( 'NONE', #6881, #10745, #5937 ) ;
#4827 = CARTESIAN_POINT ( 'NONE',  ( 27.37500000054622262, 27.65831843345427998, 90.79316153445363113 ) ) ;
#4828 = CARTESIAN_POINT ( 'NONE',  ( 20.59999999999998721, 12.86707612778636012, 88.47553407664152303 ) ) ;
#4829 = FILL_AREA_STYLE ('',( #5656 ) ) ;
#4830 = CARTESIAN_POINT ( 'NONE',  ( 35.67500000054623399, 22.36655054427230027, 98.07665518445361386 ) ) ;
#4831 = ORIENTED_EDGE ( 'NONE', *, *, #3335, .T. ) ;
#4832 = EDGE_CURVE ( 'NONE', #5989, #12402, #12210, .T. ) ;
#4833 = CARTESIAN_POINT ( 'NONE',  ( 27.49999999999999645, 20.00000000000000355, 197.9999999999999716 ) ) ;
#4834 = ORIENTED_EDGE ( 'NONE', *, *, #4474, .F. ) ;
#4835 = LINE ( 'NONE', #8821, #2661 ) ;
#4836 = ORIENTED_EDGE ( 'NONE', *, *, #3401, .T. ) ;
#4837 = VECTOR ( 'NONE', #1505, 1000.000000000000000 ) ;
#4838 = CARTESIAN_POINT ( 'NONE',  ( 43.69999999999998863, 26.37988106264029398, 95.42841645007781892 ) ) ;
#4839 = DIRECTION ( 'NONE',  ( 0.000000000000000000, 0.000000000000000000, -1.000000000000000000 ) ) ;
#4840 = CARTESIAN_POINT ( 'NONE',  ( 45.17500000054621268, 26.19570976099943849, 86.29171490190961435 ) ) ;
#4841 = CARTESIAN_POINT ( 'NONE',  ( 27.49999999999999645, 20.00000000000000355, 172.0000000000000000 ) ) ;
#4842 = CARTESIAN_POINT ( 'NONE',  ( 20.47500000054622404, 13.07298590277314432, 88.54243821818161564 ) ) ;
#4843 = CARTESIAN_POINT ( 'NONE',  ( 39.39999999999999147, 27.13292387221364876, 88.47553407664153724 ) ) ;
#4844 = CYLINDRICAL_SURFACE ( 'NONE', #6648, 10.00000000000000355 ) ;
#4845 = VECTOR ( 'NONE', #3297, 1000.000000000000114 ) ;
#4846 = VERTEX_POINT ( 'NONE', #6612 ) ;
#4847 = CARTESIAN_POINT ( 'NONE',  ( 31.95000000109245875, 13.62011893735971135, 95.42841645007781892 ) ) ;
#4848 = CARTESIAN_POINT ( 'NONE',  ( 5.022951428105686844, 11.32827475346531720, 24.49655794125914099 ) ) ;
#4849 = ORIENTED_EDGE ( 'NONE', *, *, #11066, .T. ) ;
#4850 = AXIS2_PLACEMENT_3D ( 'NONE', #793, #7832, #7645 ) ;
#4851 = ORIENTED_EDGE ( 'NONE', *, *, #8252, .T. ) ;
#4852 = CARTESIAN_POINT ( 'NONE',  ( 6.000000000000000000, -2.919948986426523341, 5.057500000000002771 ) ) ;
#4853 = DIRECTION ( 'NONE',  ( -1.000000000000000000, -0.000000000000000000, -0.000000000000000000 ) ) ;
#4854 = CARTESIAN_POINT ( 'NONE',  ( -5.303430480311382311, 28.48399989248413178, 24.43255084236253794 ) ) ;
#4855 = AXIS2_PLACEMENT_3D ( 'NONE', #9928, #10055, #8972 ) ;
#4856 = CARTESIAN_POINT ( 'NONE',  ( 38.87500000054623683, 22.36655054427230382, 83.50966788445364841 ) ) ;
#4857 = CARTESIAN_POINT ( 'NONE',  ( 36.37500000054623683, 12.34168156654572535, 90.79316153445363113 ) ) ;
#4858 = CARTESIAN_POINT ( 'NONE',  ( -4.140053538423851224E-16, 30.00000000000001066, -28.00000000000000355 ) ) ;
#4859 = CARTESIAN_POINT ( 'NONE',  ( 34.05000000109246372, 12.86707612778636012, 93.11078899226572503 ) ) ;
#4860 = ORIENTED_EDGE ( 'NONE', *, *, #4791, .F. ) ;
#4861 = CARTESIAN_POINT ( 'NONE',  ( 3.050334177726442775, 53.97519422362026376, -27.83468959413792732 ) ) ;
#4862 = CARTESIAN_POINT ( 'NONE',  ( 5.340684424226280325E-17, 55.00000000000000000, -25.00000000000000000 ) ) ;
#4863 = CARTESIAN_POINT ( 'NONE',  ( 31.03600000000003689, 7.347880794884123680E-16, -6.000000000000003553 ) ) ;
#4864 = ORIENTED_EDGE ( 'NONE', *, *, #6827, .F. ) ;
#4865 = EDGE_CURVE ( 'NONE', #3559, #7152, #12456, .T. ) ;
#4866 = CARTESIAN_POINT ( 'NONE',  ( -50.00000000000001421, 22.00000000000000000, 152.2284161474004520 ) ) ;
#4867 = CARTESIAN_POINT ( 'NONE',  ( -3.594513446512490388E-16, 55.00000000000000000, -21.00000000000000000 ) ) ;
#4868 = ORIENTED_EDGE ( 'NONE', *, *, #1553, .T. ) ;
#4869 = ORIENTED_EDGE ( 'NONE', *, *, #11716, .F. ) ;
#4870 = CARTESIAN_POINT ( 'NONE',  ( -6.854073901798486190, 27.28868271418044245, -19.85144179826269450 ) ) ;
#4871 = AXIS2_PLACEMENT_3D ( 'NONE', #8773, #11759, #221 ) ;
#4872 = CARTESIAN_POINT ( 'NONE',  ( -5.000000000000000000, 50.00000000000000000, -28.00000000000000711 ) ) ;
#4873 = CARTESIAN_POINT ( 'NONE',  ( 10.00000000000000355, 20.00000000000000355, 83.29316153445363113 ) ) ;
#4874 = DIRECTION ( 'NONE',  ( 0.000000000000000000, 1.000000000000000000, 0.000000000000000000 ) ) ;
#4875 = CARTESIAN_POINT ( 'NONE',  ( -4.831180326583886853, 51.29868641109617755, -20.43678301931617014 ) ) ;
#4876 = CARTESIAN_POINT ( 'NONE',  ( -8.665812433443574132E-16, 55.00000000000000000, -28.00000000000000355 ) ) ;
#4877 = CARTESIAN_POINT ( 'NONE',  ( 9.671223021026712274, 22.62837036926845968, -18.64106995571668079 ) ) ;
#4878 = CYLINDRICAL_SURFACE ( 'NONE', #5286, 10.00000000000000355 ) ;
#4879 = ORIENTED_EDGE ( 'NONE', *, *, #5104, .F. ) ;
#4880 = CIRCLE ( 'NONE', #10737, 6.999999999999978684 ) ;
#4881 = CARTESIAN_POINT ( 'NONE',  ( 1.651856453710261352, 29.86806670974593914, -24.94744891504881679 ) ) ;
#4882 = EDGE_CURVE ( 'NONE', #378, #11906, #1792, .T. ) ;
#4883 = ITEM_DEFINED_TRANSFORMATION ( 'NONE', 'NONE', #9808,  #9021 ) ;
#4884 = CARTESIAN_POINT ( 'NONE',  ( 21.17500000054622689, 26.19570976099943849, 86.29171490190961435 ) ) ;
#4885 = CARTESIAN_POINT ( 'NONE',  ( 49.27500000054622120, 26.92701409722686634, 88.54243821818162985 ) ) ;
#4886 = ADVANCED_FACE ( 'NONE', ( #3573 ), #7448, .F. ) ;
#4887 = CARTESIAN_POINT ( 'NONE',  ( 41.07500000054622546, 26.19570976099943849, 86.29171490190961435 ) ) ;
#4888 = CARTESIAN_POINT ( 'NONE',  ( 26.57500000054622191, 13.80429023900056684, 86.29171490190961435 ) ) ;
#4889 = CARTESIAN_POINT ( 'NONE',  ( 22.49999999999998934, 12.11403331821300533, 90.79316153445363113 ) ) ;
#4890 = CIRCLE ( 'NONE', #1246, 10.00000000000000355 ) ;
#4891 = CARTESIAN_POINT ( 'NONE',  ( 34.10000000000000142, 17.56310227825320425, 98.29316153445363113 ) ) ;
#4892 = CARTESIAN_POINT ( 'NONE',  ( 31.67500000054622689, 22.36655054427230027, 98.07665518445361386 ) ) ;
#4893 = ORIENTED_EDGE ( 'NONE', *, *, #5139, .F. ) ;
#4894 = FACE_OUTER_BOUND ( 'NONE', #6222, .T. ) ;
#4895 = VERTEX_POINT ( 'NONE', #3512 ) ;
#4896 = CARTESIAN_POINT ( 'NONE',  ( 49.25000000109246656, 27.13292387221364876, 93.11078899226573924 ) ) ;
#4897 = ORIENTED_EDGE ( 'NONE', *, *, #9100, .T. ) ;
#4898 = SHAPE_REPRESENTATION_RELATIONSHIP ( 'NONE' , 'NONE' ,  #7408, #7483 ) ;
#4899 = CARTESIAN_POINT ( 'NONE',  ( 32.19999999999999574, 15.59161060780645691, 96.86078899226572503 ) ) ;
#4900 = DIRECTION ( 'NONE',  ( 1.000000000000000000, -0.000000000000000000, -0.000000000000000000 ) ) ;
#4901 = ADVANCED_BREP_SHAPE_REPRESENTATION ( '', ( #2081, #9021 ), #2935 ) ;
#4902 = CARTESIAN_POINT ( 'NONE',  ( 46.07500000054622546, 15.71886984736413417, 96.68563167572563088 ) ) ;
#4903 = PLANE ( 'NONE',  #4930 ) ;
#4904 = EDGE_CURVE ( 'NONE', #7736, #1411, #5553, .T. ) ;
#4905 = CARTESIAN_POINT ( 'NONE',  ( 5.000000000000000000, 2.342598717236900718, -4.057500000000001883 ) ) ;
#4906 = CARTESIAN_POINT ( 'NONE',  ( 45.07500000054622546, 24.28113015263587471, 84.90069139318163138 ) ) ;
#4907 = CARTESIAN_POINT ( 'NONE',  ( 42.29999999999998295, 13.62011893735971135, 95.42841645007781892 ) ) ;
#4908 = CARTESIAN_POINT ( 'NONE',  ( 45.29999999999999005, 26.37988106264029398, 86.15790661882942914 ) ) ;
#4909 = PLANE ( 'NONE',  #6443 ) ;
#4910 = ORIENTED_EDGE ( 'NONE', *, *, #2420, .F. ) ;
#4911 = CARTESIAN_POINT ( 'NONE',  ( 33.75000000109246656, 17.56310227825320425, 98.29316153445363113 ) ) ;
#4912 = CARTESIAN_POINT ( 'NONE',  ( 3.241086154805254083, 10.53405487867120982, 24.79105057270042067 ) ) ;
#4913 = ORIENTED_EDGE ( 'NONE', *, *, #9568, .T. ) ;
#4914 = ADVANCED_FACE ( 'NONE', ( #7511 ), #4714, .F. ) ;
#4915 = ORIENTED_EDGE ( 'NONE', *, *, #11465, .F. ) ;
#4916 = CARTESIAN_POINT ( 'NONE',  ( -2.610103423518925769, 29.65902056345734650, -24.86541183722168213 ) ) ;
#4917 = CARTESIAN_POINT ( 'NONE',  ( -4.743369866101525112, 51.61445767325203349, -24.54621253249761637 ) ) ;
#4918 = DIRECTION ( 'NONE',  ( -1.000000000000000000, 0.000000000000000000, 0.000000000000000000 ) ) ;
#4919 = CARTESIAN_POINT ( 'NONE',  ( 36.77500000054622831, 20.00000000000000355, 83.50966788445364841 ) ) ;
#4920 = CARTESIAN_POINT ( 'NONE',  ( 30.57500000054622191, 13.80429023900056684, 86.29171490190961435 ) ) ;
#4921 = AXIS2_PLACEMENT_3D ( 'NONE', #10102, #8076, #7114 ) ;
#4922 = CARTESIAN_POINT ( 'NONE',  ( -9.670693212272151840, 22.62952413424389420, 18.64134173399714811 ) ) ;
#4923 = CARTESIAN_POINT ( 'NONE',  ( 92.00000000000000000, 0.000000000000000000, 0.000000000000000000 ) ) ;
#4924 = ORIENTED_EDGE ( 'NONE', *, *, #6560, .T. ) ;
#4925 = FACE_BOUND ( 'NONE', #4193, .T. ) ;
#4926 = ORIENTED_EDGE ( 'NONE', *, *, #8399, .F. ) ;
#4927 = CARTESIAN_POINT ( 'NONE',  ( 46.65000000109246514, 20.00000000000000355, 83.29316153445364534 ) ) ;
#4928 = ORIENTED_EDGE ( 'NONE', *, *, #189, .F. ) ;
#4929 = ORIENTED_EDGE ( 'NONE', *, *, #10015, .T. ) ;
#4930 = AXIS2_PLACEMENT_3D ( 'NONE', #8763, #1099, #3306 ) ;
#4931 = LINE ( 'NONE', #8927, #1554 ) ;
#4932 = CARTESIAN_POINT ( 'NONE',  ( 8.248483781669884607, 25.66706883268630079, 85.85796419627257592 ) ) ;
#4933 = CARTESIAN_POINT ( 'NONE',  ( 37.59999999999998721, 27.13292387221364876, 93.11078899226573924 ) ) ;
#4934 = AXIS2_PLACEMENT_3D ( 'NONE', #10685, #10886, #4990 ) ;
#4935 = CARTESIAN_POINT ( 'NONE',  ( -4.967147891453746134, 49.34082981697670078, -24.50166768924217564 ) ) ;
#4936 = FACE_OUTER_BOUND ( 'NONE', #8651, .T. ) ;
#4937 = CARTESIAN_POINT ( 'NONE',  ( 26.55000000109246372, 17.56310227825324333, 83.29316153445360271 ) ) ;
#4938 = AXIS2_PLACEMENT_3D ( 'NONE', #9579, #1829, #8499 ) ;
#4939 = CARTESIAN_POINT ( 'NONE',  ( -28.50000000000001066, 77.00000000000000000, 166.8533255156881694 ) ) ;
#4940 = ORIENTED_EDGE ( 'NONE', *, *, #10326, .T. ) ;
#4941 = CARTESIAN_POINT ( 'NONE',  ( 8.964356567778166252, 24.44381301785154292, -23.33811713236289620 ) ) ;
#4942 = ITEM_DEFINED_TRANSFORMATION ( 'NONE', 'NONE', #10603,  #9021 ) ;
#4943 = AXIS2_PLACEMENT_3D ( 'NONE', #12527, #1926, #11578 ) ;
#4944 = EDGE_CURVE ( 'NONE', #11614, #9971, #7661, .T. ) ;
#4945 = VECTOR ( 'NONE', #2464, 1000.000000000000000 ) ;
#4946 = CARTESIAN_POINT ( 'NONE',  ( 23.77500000054622475, 22.36655054427230027, 98.07665518445361386 ) ) ;
#4947 = CARTESIAN_POINT ( 'NONE',  ( 24.15000000109246159, 12.11403331821300533, 90.79316153445363113 ) ) ;
#4948 = CARTESIAN_POINT ( 'NONE',  ( 35.57500000054622546, 24.28113015263587116, 96.68563167572563088 ) ) ;
#4949 = CARTESIAN_POINT ( 'NONE',  ( 2.620611987601386250, 10.32688167823381953, -24.87076294850758984 ) ) ;
#4950 = CARTESIAN_POINT ( 'NONE',  ( 20.39999999999998792, 12.86707612778636012, 93.11078899226572503 ) ) ;
#4951 = EDGE_CURVE ( 'NONE', #11209, #7418, #5114, .T. ) ;
#4952 = CARTESIAN_POINT ( 'NONE',  ( 3.061616997868383043E-15, 0.000000000000000000, 25.00000000000000000 ) ) ;
#4953 = CARTESIAN_POINT ( 'NONE',  ( 29.97500000054622760, 15.71886984736413417, 96.68563167572563088 ) ) ;
#4954 = EDGE_LOOP ( 'NONE', ( #3214, #2482 ) ) ;
#4955 = DIRECTION ( 'NONE',  ( -0.000000000000000000, 0.000000000000000000, 1.000000000000000000 ) ) ;
#4956 = ORIENTED_EDGE ( 'NONE', *, *, #6821, .F. ) ;
#4957 = VECTOR ( 'NONE', #2071, 1000.000000000000000 ) ;
#4958 = CARTESIAN_POINT ( 'NONE',  ( 4.999999999999999112, 18.00000000000000355, 218.7511230907454944 ) ) ;
#4959 = ORIENTED_EDGE ( 'NONE', *, *, #9521, .F. ) ;
#4960 =( BOUNDED_CURVE ( )  B_SPLINE_CURVE ( 2, ( #7754, #3187, #4965, #211, #3119, #3944, #1166, #81, #11881, #10788, #7820 ),
 .UNSPECIFIED., .F., .F. ) 
 B_SPLINE_CURVE_WITH_KNOTS ( ( 3, 2, 2, 2, 2, 3 ),
 ( 0.2999999999999999889, 0.3066666666666666430, 0.3133333333333333526, 0.3200000000000000622, 0.3266666666666667163, 0.3333333333333333703 ),
 .UNSPECIFIED. ) 
 CURVE ( )  GEOMETRIC_REPRESENTATION_ITEM ( )  RATIONAL_B_SPLINE_CURVE ( ( 1.000000000000000000, 0.9510565162951535312, 1.000000000000000000, 0.9510565162951535312, 1.000000000000000000, 0.9510565162951535312, 1.000000000000000000, 0.9510565162951535312, 1.000000000000000000, 0.9510565162951530871, 1.000000000000000444 ) ) 
 REPRESENTATION_ITEM ( '' )  );
#4961 = PLANE ( 'NONE',  #2540 ) ;
#4962 = CARTESIAN_POINT ( 'NONE',  ( 9.917745391744515970, 18.67758101133046722, -26.18472015824584531 ) ) ;
#4963 = ADVANCED_FACE ( 'NONE', ( #7574 ), #11503, .F. ) ;
#4964 = CARTESIAN_POINT ( 'NONE',  ( 36.27500000054622120, 13.07298590277314254, 93.04388485072563242 ) ) ;
#4965 = CARTESIAN_POINT ( 'NONE',  ( 40.45000000109246940, 15.59161060780646046, 84.72553407664153724 ) ) ;
#4966 = DIRECTION ( 'NONE',  ( 0.000000000000000000, 0.000000000000000000, -1.000000000000000000 ) ) ;
#4967 = CARTESIAN_POINT ( 'NONE',  ( 37.17500000054620557, 26.19570976099943493, 86.29171490190961435 ) ) ;
#4968 = CARTESIAN_POINT ( 'NONE',  ( 42.99999999999999289, 20.00000000000000355, 83.29316153445364534 ) ) ;
#4969 = CIRCLE ( 'NONE', #12064, 6.000000000000003553 ) ;
#4970 = EDGE_CURVE ( 'NONE', #7888, #5428, #6726, .T. ) ;
#4971 = CARTESIAN_POINT ( 'NONE',  ( 39.09999999999999432, 22.43689772174678509, 83.29316153445363113 ) ) ;
#4972 = ORIENTED_EDGE ( 'NONE', *, *, #10366, .F. ) ;
#4973 = APPLICATION_CONTEXT ( 'automotive_design' ) ;
#4974 = CARTESIAN_POINT ( 'NONE',  ( 30.45000000109246585, 15.59161060780646046, 84.72553407664153724 ) ) ;
#4975 = CARTESIAN_POINT ( 'NONE',  ( -31.74999999999995737, 0.000000000000000000, 9.000000000000000000 ) ) ;
#4976 = ORIENTED_EDGE ( 'NONE', *, *, #6815, .F. ) ;
#4977 = ADVANCED_FACE ( 'NONE', ( #3064 ), #4909, .F. ) ;
#4978 = ORIENTED_EDGE ( 'NONE', *, *, #4161, .F. ) ;
#4979 = PLANE ( 'NONE',  #5471 ) ;
#4980 = PLANE ( 'NONE',  #6429 ) ;
#4981 = DIRECTION ( 'NONE',  ( -0.000000000000000000, -1.000000000000000000, -0.000000000000000000 ) ) ;
#4982 = ADVANCED_FACE ( 'NONE', ( #4010 ), #4844, .F. ) ;
#4983 = CARTESIAN_POINT ( 'NONE',  ( 32.37500000054622973, 13.07298590277314432, 88.54243821818161564 ) ) ;
#4984 = CARTESIAN_POINT ( 'NONE',  ( 30.07500000054622546, 15.71886984736413417, 96.68563167572563088 ) ) ;
#4985 = CARTESIAN_POINT ( 'NONE',  ( -2.216580177477698310, 54.48481978330000430, 27.91250211204058473 ) ) ;
#4986 = DIRECTION ( 'NONE',  ( 1.000000000000000000, 0.000000000000000000, 0.000000000000000000 ) ) ;
#4987 = DIRECTION ( 'NONE',  ( -0.000000000000000000, -0.000000000000000000, 1.000000000000000000 ) ) ;
#4988 = ORIENTED_EDGE ( 'NONE', *, *, #9025, .F. ) ;
#4989 = CARTESIAN_POINT ( 'NONE',  ( 48.67500000054622689, 15.71886984736413773, 84.90069139318163138 ) ) ;
#4990 = DIRECTION ( 'NONE',  ( 0.000000000000000000, -1.224646799147353454E-16, 1.000000000000000000 ) ) ;
#4991 = DIRECTION ( 'NONE',  ( 0.000000000000000000, 0.000000000000000000, -1.000000000000000000 ) ) ;
#4992 = EDGE_LOOP ( 'NONE', ( #3035, #9305, #5494, #5554, #1280, #11685 ) ) ;
#4993 = CARTESIAN_POINT ( 'NONE',  ( -34.99999999999999289, 24.39339828220178674, 137.5000000000000000 ) ) ;
#4994 = EDGE_CURVE ( 'NONE', #1035, #9150, #9859, .T. ) ;
#4995 = ORIENTED_EDGE ( 'NONE', *, *, #4585, .T. ) ;
#4996 = DIRECTION ( 'NONE',  ( 0.000000000000000000, 0.000000000000000000, 1.000000000000000000 ) ) ;
#4997 = ORIENTED_EDGE ( 'NONE', *, *, #1944, .T. ) ;
#4998 = DIRECTION ( 'NONE',  ( 0.000000000000000000, 0.000000000000000000, 1.000000000000000000 ) ) ;
#4999 = DIRECTION ( 'NONE',  ( 0.000000000000000000, -0.5000000000000012212, -0.8660254037844380415 ) ) ;
#5000 = CARTESIAN_POINT ( 'NONE',  ( -21.00000000000001066, 77.00000000000000000, 154.3533255156881978 ) ) ;
#5001 = DIRECTION ( 'NONE',  ( 1.000000000000000000, 0.000000000000000000, 0.000000000000000000 ) ) ;
#5002 = DIRECTION ( 'NONE',  ( 0.000000000000000000, 0.000000000000000000, 1.000000000000000000 ) ) ;
#5003 = CARTESIAN_POINT ( 'NONE',  ( -2.000000000000015543, 20.00000000000000355, 83.29316153445364534 ) ) ;
#5004 = CARTESIAN_POINT ( 'NONE',  ( 1.343687355773163672, 29.93123645385455944, -20.96702215260311064 ) ) ;
#5005 = CARTESIAN_POINT ( 'NONE',  ( 40.97500000054622404, 24.28113015263587471, 84.90069139318163138 ) ) ;
#5006 = CARTESIAN_POINT ( 'NONE',  ( 3.548862490157215444, 10.64523530928737749, 24.74869899623665503 ) ) ;
#5007 = ORIENTED_EDGE ( 'NONE', *, *, #3037, .T. ) ;
#5008 = CARTESIAN_POINT ( 'NONE',  ( 9.935507569286025742, 21.31398369048515562, -22.94135581966985526 ) ) ;
#5009 = CONTEXT_DEPENDENT_SHAPE_REPRESENTATION ( #7393, #10848 ) ;
#5010 = CIRCLE ( 'NONE', #8856, 5.400000000000001243 ) ;
#5011 = CARTESIAN_POINT ( 'NONE',  ( 23.87500000054622262, 20.00000000000000355, 98.07665518445361386 ) ) ;
#5012 = CARTESIAN_POINT ( 'NONE',  ( -6.999999999999999112, 77.00000000000000000, 101.8533255156881978 ) ) ;
#5013 = CARTESIAN_POINT ( 'NONE',  ( 32.47500000054623115, 13.80429023900056684, 86.29171490190961435 ) ) ;
#5014 = CARTESIAN_POINT ( 'NONE',  ( 22.57500000054622546, 13.80429023900056684, 86.29171490190961435 ) ) ;
#5015 = CARTESIAN_POINT ( 'NONE',  ( 21.09999999999998010, 22.43689772174679575, 83.29316153445363113 ) ) ;
#5016 = CARTESIAN_POINT ( 'NONE',  ( 3.429011038972528284E-15, 30.00000000000001066, 28.00000000000000355 ) ) ;
#5017 = CARTESIAN_POINT ( 'NONE',  ( 33.17500000054622689, 26.92701409722686634, 88.54243821818162985 ) ) ;
#5018 = EDGE_LOOP ( 'NONE', ( #7627, #9468, #10483, #3518, #2467, #4211 ) ) ;
#5019 = CARTESIAN_POINT ( 'NONE',  ( 6.955575927950914131E-22, 45.00000000000000711, -25.00000000000000000 ) ) ;
#5020 = PLANE ( 'NONE',  #1529 ) ;
#5021 = VECTOR ( 'NONE', #10249, 1000.000000000000000 ) ;
#5022 = ORIENTED_EDGE ( 'NONE', *, *, #919, .T. ) ;
#5023 = ADVANCED_FACE ( 'NONE', ( #3950, #153 ), #7826, .T. ) ;
#5024 = CARTESIAN_POINT ( 'NONE',  ( 48.75000000109245946, 22.43689772174678509, 83.29316153445363113 ) ) ;
#5025 = ORIENTED_EDGE ( 'NONE', *, *, #9864, .F. ) ;
#5026 =( NAMED_UNIT ( * ) SI_UNIT ( $, .STERADIAN. ) SOLID_ANGLE_UNIT ( ) );
#5027 = CARTESIAN_POINT ( 'NONE',  ( 20.65000000109246514, 20.00000000000000355, 83.29316153445364534 ) ) ;
#5028 = CARTESIAN_POINT ( 'NONE',  ( 0.6563718250326410208, 10.01611854420673708, -27.99423098641389629 ) ) ;
#5029 = AXIS2_PLACEMENT_3D ( 'NONE', #7966, #11834, #6752 ) ;
#5030 = CARTESIAN_POINT ( 'NONE',  ( 40.97500000054621694, 22.36655054427230382, 83.50966788445364841 ) ) ;
#5031 = LINE ( 'NONE', #8960, #63 ) ;
#5032 = CARTESIAN_POINT ( 'NONE',  ( 40.07500000054623257, 15.71886984736413417, 96.68563167572563088 ) ) ;
#5033 = CARTESIAN_POINT ( 'NONE',  ( 40.69999999999999574, 13.62011893735971135, 86.15790661882942914 ) ) ;
#5034 = CARTESIAN_POINT ( 'NONE',  ( 45.89999999999999147, 22.43689772174683128, 98.29316153445361692 ) ) ;
#5035 = FACE_OUTER_BOUND ( 'NONE', #6789, .T. ) ;
#5036 = VERTEX_POINT ( 'NONE', #1172 ) ;
#5037 = CARTESIAN_POINT ( 'NONE',  ( 28.35000000109246443, 13.62011893735971135, 86.15790661882942914 ) ) ;
#5038 = PLANE ( 'NONE',  #10955 ) ;
#5039 = ORIENTED_EDGE ( 'NONE', *, *, #1653, .F. ) ;
#5040 =( BOUNDED_CURVE ( )  B_SPLINE_CURVE ( 2, ( #6091, #2282, #5901, #5141, #9009, #8746, #1080, #8810, #129, #3988, #7865 ),
 .UNSPECIFIED., .F., .F. ) 
 B_SPLINE_CURVE_WITH_KNOTS ( ( 3, 2, 2, 2, 2, 3 ),
 ( 0.1000000000000000888, 0.1066666666666667568, 0.1133333333333334247, 0.1200000000000000927, 0.1266666666666667884, 0.1333333333333334425 ),
 .UNSPECIFIED. ) 
 CURVE ( )  GEOMETRIC_REPRESENTATION_ITEM ( )  RATIONAL_B_SPLINE_CURVE ( ( 0.9999999999999994449, 0.9510565162951540863, 1.000000000000000000, 0.9510565162951535312, 1.000000000000000000, 0.9510565162951535312, 1.000000000000000000, 0.9510565162951535312, 1.000000000000000000, 0.9510565162951527540, 1.000000000000000888 ) ) 
 REPRESENTATION_ITEM ( '' )  );
#5041 = AXIS2_PLACEMENT_3D ( 'NONE', #1957, #191, #7798 ) ;
#5042 = EDGE_LOOP ( 'NONE', ( #9489, #3253, #2782, #7875 ) ) ;
#5043 = PRESENTATION_LAYER_ASSIGNMENT (  '', '', ( #9498 ) ) ;
#5044 = LINE ( 'NONE', #6120, #8704 ) ;
#5045 = EDGE_CURVE ( 'NONE', #2352, #10270, #8768, .T. ) ;
#5046 = CARTESIAN_POINT ( 'NONE',  ( -3.767068525368503895, 53.30379312071067233, -24.71564595051174607 ) ) ;
#5047 = DIRECTION ( 'NONE',  ( 1.000000000000000000, 0.000000000000000000, 0.000000000000000000 ) ) ;
#5048 = AXIS2_PLACEMENT_3D ( 'NONE', #2937, #3885, #7760 ) ;
#5049 = CARTESIAN_POINT ( 'NONE',  ( 30.67500000054622689, 17.63344945572770328, 83.50966788445364841 ) ) ;
#5050 = CARTESIAN_POINT ( 'NONE',  ( 29.67500000054622333, 24.28113015263587116, 96.68563167572563088 ) ) ;
#5051 = CARTESIAN_POINT ( 'NONE',  ( 0.000000000000000000, 0.000000000000000000, -25.00000000000000000 ) ) ;
#5052 = CARTESIAN_POINT ( 'NONE',  ( 9.660207172539163167, 22.60549549288601412, -26.28099775896728829 ) ) ;
#5053 = CARTESIAN_POINT ( 'NONE',  ( 33.65000000109246514, 20.00000000000000355, 98.29316153445363113 ) ) ;
#5054 = ORIENTED_EDGE ( 'NONE', *, *, #2174, .T. ) ;
#5055 = CARTESIAN_POINT ( 'NONE',  ( 49.35000000109246798, 26.37988106264029398, 95.42841645007781892 ) ) ;
#5056 = CARTESIAN_POINT ( 'NONE',  ( -10.00000000000000355, 20.00000000000000355, -22.91287847477919826 ) ) ;
#5057 = ORIENTED_EDGE ( 'NONE', *, *, #4665, .F. ) ;
#5058 = DIRECTION ( 'NONE',  ( 1.000000000000000000, 0.000000000000000000, 0.000000000000000000 ) ) ;
#5059 = ORIENTED_EDGE ( 'NONE', *, *, #1857, .T. ) ;
#5060 = AXIS2_PLACEMENT_3D ( 'NONE', #3423, #4310, #632 ) ;
#5061 = CARTESIAN_POINT ( 'NONE',  ( -33.79382810696421302, 14.62220435867159374, 151.2938281069642130 ) ) ;
#5062 = CARTESIAN_POINT ( 'NONE',  ( -8.664197377259947430, 14.96499702975700608, -23.45374477514955203 ) ) ;
#5063 = CIRCLE ( 'NONE', #12149, 5.999999999999998224 ) ;
#5064 = DIRECTION ( 'NONE',  ( 0.000000000000000000, 0.000000000000000000, -1.000000000000000000 ) ) ;
#5065 = CARTESIAN_POINT ( 'NONE',  ( -4.140053538423851224E-16, 30.00000000000001066, -28.00000000000000355 ) ) ;
#5066 = ADVANCED_FACE ( 'NONE', ( #11694 ), #7952, .F. ) ;
#5067 = CARTESIAN_POINT ( 'NONE',  ( 8.962237153663121347, 24.44132309231766698, 84.74490591176112275 ) ) ;
#5068 = CARTESIAN_POINT ( 'NONE',  ( 6.000000000000000000, 8.759846959279592227, -5.057500000000009877 ) ) ;
#5069 = CARTESIAN_POINT ( 'NONE',  ( -4.329834338986901621, 47.49413952373966197, -24.62232128246942509 ) ) ;
#5070 = CARTESIAN_POINT ( 'NONE',  ( -3.709758735690515970E-18, 30.00000000000001066, -25.00000000000000000 ) ) ;
#5071 = CARTESIAN_POINT ( 'NONE',  ( -3.973686166794720975, 46.94757989445042767, 27.71721093970095495 ) ) ;
#5072 = CARTESIAN_POINT ( 'NONE',  ( 45.07500000054621836, 26.19570976099943493, 86.29171490190961435 ) ) ;
#5073 = DIRECTION ( 'NONE',  ( -0.000000000000000000, -0.000000000000000000, -1.000000000000000000 ) ) ;
#5074 = VERTEX_POINT ( 'NONE', #3000 ) ;
#5075 = ADVANCED_FACE ( 'NONE', ( #10669 ), #10731, .T. ) ;
#5076 = LINE ( 'NONE', #7737, #12126 ) ;
#5077 = AXIS2_PLACEMENT_3D ( 'NONE', #11305, #9533, #6419 ) ;
#5078 = CARTESIAN_POINT ( 'NONE',  ( 22.87500000054622618, 20.00000000000000355, 83.50966788445364841 ) ) ;
#5079 = CARTESIAN_POINT ( 'NONE',  ( 48.47500000054622404, 13.07298590277314432, 88.54243821818161564 ) ) ;
#5080 = CARTESIAN_POINT ( 'NONE',  ( 31.07500000054622546, 26.19570976099943849, 86.29171490190961435 ) ) ;
#5081 = CARTESIAN_POINT ( 'NONE',  ( 23.97500000054622049, 17.63344945572769973, 98.07665518445361386 ) ) ;
#5082 = CARTESIAN_POINT ( 'NONE',  ( 20.99999999999998579, 20.00000000000000355, 83.29316153445364534 ) ) ;
#5083 = LINE ( 'NONE', #1275, #5458 ) ;
#5084 = CARTESIAN_POINT ( 'NONE',  ( 28.67500000054623044, 17.63344945572770328, 83.50966788445364841 ) ) ;
#5085 = EDGE_LOOP ( 'NONE', ( #1191, #11076, #3447, #586, #4702 ) ) ;
#5086 = PRODUCT ( 'Bearing Block Mounting Shaft', 'Bearing Block Mounting Shaft', '', ( #9769 ) ) ;
#5087 = CARTESIAN_POINT ( 'NONE',  ( 33.55000000109246372, 22.43689772174679575, 98.29316153445363113 ) ) ;
#5088 = EDGE_LOOP ( 'NONE', ( #5679, #4469, #1234, #7909, #2924 ) ) ;
#5089 = CARTESIAN_POINT ( 'NONE',  ( 4.832070635542911496, 51.29541901974291562, 27.57994638421516242 ) ) ;
#5090 = VERTEX_POINT ( 'NONE', #9793 ) ;
#5091 = CARTESIAN_POINT ( 'NONE',  ( 10.00000000000000355, 20.00000000000000355, -28.00000000000000711 ) ) ;
#5092 = VECTOR ( 'NONE', #8635, 1000.000000000000000 ) ;
#5093 = CARTESIAN_POINT ( 'NONE',  ( 35.37500000054622973, 27.65831843345427998, 90.79316153445363113 ) ) ;
#5094 = DIRECTION ( 'NONE',  ( -1.000000000000000000, 0.000000000000000000, 0.000000000000000000 ) ) ;
#5095 = EDGE_CURVE ( 'NONE', #5215, #8335, #9299, .T. ) ;
#5096 = CARTESIAN_POINT ( 'NONE',  ( 20.55000000109246372, 17.56310227825320425, 83.29316153445363113 ) ) ;
#5097 = CARTESIAN_POINT ( 'NONE',  ( 39.17500000054621978, 26.19570976099943493, 86.29171490190961435 ) ) ;
#5098 = CARTESIAN_POINT ( 'NONE',  ( 44.39999999999999147, 12.86707612778636012, 93.11078899226572503 ) ) ;
#5099 = CARTESIAN_POINT ( 'NONE',  ( 46.87500000054622262, 22.36655054427230382, 83.50966788445364841 ) ) ;
#5100 = ORIENTED_EDGE ( 'NONE', *, *, #4336, .T. ) ;
#5101 = CARTESIAN_POINT ( 'NONE',  ( 28.75000000109245946, 22.43689772174679575, 83.29316153445363113 ) ) ;
#5102 = CARTESIAN_POINT ( 'NONE',  ( 3.303834617765012194, 46.23291288788979614, -24.78182658752202983 ) ) ;
#5103 = ORIENTED_EDGE ( 'NONE', *, *, #11448, .F. ) ;
#5104 = EDGE_CURVE ( 'NONE', #5277, #3559, #1978, .T. ) ;
#5105 = FACE_OUTER_BOUND ( 'NONE', #5682, .T. ) ;
#5106 = ORIENTED_EDGE ( 'NONE', *, *, #4009, .T. ) ;
#5107 = CARTESIAN_POINT ( 'NONE',  ( 0.6590680265247156333, 9.999999999999994671, 28.00000000000000355 ) ) ;
#5108 = DIRECTION ( 'NONE',  ( 0.000000000000000000, 1.000000000000000000, -1.039664082171044875E-15 ) ) ;
#5109 = DIRECTION ( 'NONE',  ( 1.000000000000000000, -0.000000000000000000, -0.000000000000000000 ) ) ;
#5110 = PRODUCT_DEFINITION_CONTEXT ( 'detailed design', #11049, 'design' ) ;
#5111 = EDGE_CURVE ( 'NONE', #10641, #2251, #8041, .T. ) ;
#5112 = CARTESIAN_POINT ( 'NONE',  ( 29.57500000054622546, 24.28113015263587116, 96.68563167572563088 ) ) ;
#5113 = CARTESIAN_POINT ( 'NONE',  ( 32.17500000054621978, 13.80429023900056507, 95.29460816699764791 ) ) ;
#5114 =( BOUNDED_CURVE ( )  B_SPLINE_CURVE ( 2, ( #10420, #4528, #784, #5493, #7384, #9548, #2811, #8523, #3694, #3758, #7638 ),
 .UNSPECIFIED., .F., .F. ) 
 B_SPLINE_CURVE_WITH_KNOTS ( ( 3, 2, 2, 2, 2, 3 ),
 ( 0.3333333333333333703, 0.3400000000000000799, 0.3466666666666667340, 0.3533333333333333881, 0.3600000000000000422, 0.3666666666666666963 ),
 .UNSPECIFIED. ) 
 CURVE ( )  GEOMETRIC_REPRESENTATION_ITEM ( )  RATIONAL_B_SPLINE_CURVE ( ( 0.9999999999999995559, 0.9510565162951539753, 1.000000000000000000, 0.9510565162951535312, 1.000000000000000000, 0.9510565162951535312, 1.000000000000000000, 0.9510565162951535312, 1.000000000000000000, 0.9510565162951530871, 1.000000000000000444 ) ) 
 REPRESENTATION_ITEM ( '' )  );
#5115 = CARTESIAN_POINT ( 'NONE',  ( 2.286292697989654954, 29.74065845437095490, -27.90836410094387787 ) ) ;
#5116 = ORIENTED_EDGE ( 'NONE', *, *, #11659, .F. ) ;
#5117 = ADVANCED_FACE ( 'NONE', ( #5035 ), #10217, .F. ) ;
#5118 = CARTESIAN_POINT ( 'NONE',  ( 47.87500000054622262, 20.00000000000000355, 98.07665518445361386 ) ) ;
#5119 = CARTESIAN_POINT ( 'NONE',  ( 48.15000000109246514, 12.11403331821300533, 90.79316153445363113 ) ) ;
#5120 = DIRECTION ( 'NONE',  ( -1.000000000000000000, 0.000000000000000000, 0.000000000000000000 ) ) ;
#5121 = ORIENTED_EDGE ( 'NONE', *, *, #1502, .F. ) ;
#5122 = DIRECTION ( 'NONE',  ( 0.000000000000000000, -0.000000000000000000, 1.000000000000000000 ) ) ;
#5123 = ORIENTED_EDGE ( 'NONE', *, *, #720, .T. ) ;
#5124 = PRODUCT_DEFINITION ( 'UNKNOWN', '', #3117, #289 ) ;
#5125 = CARTESIAN_POINT ( 'NONE',  ( -2.300052248552254319, 10.26239894176076994, -20.87624245596524730 ) ) ;
#5126 = EDGE_CURVE ( 'NONE', #8822, #8125, #6455, .T. ) ;
#5127 = CARTESIAN_POINT ( 'NONE',  ( 0.000000000000000000, 50.00000000000000000, -28.00000000000000711 ) ) ;
#5128 = CARTESIAN_POINT ( 'NONE',  ( 34.72841614740047333, 22.00000000000000000, 152.2284161474004520 ) ) ;
#5129 = CARTESIAN_POINT ( 'NONE',  ( 9.682803526473488631, 22.51080964628191339, 83.72143117422299952 ) ) ;
#5130 = CARTESIAN_POINT ( 'NONE',  ( 49.99999999999998579, 0.000000000000000000, 169.9999999999999716 ) ) ;
#5131 = CARTESIAN_POINT ( 'NONE',  ( 0.000000000000000000, 0.000000000000000000, 0.000000000000000000 ) ) ;
#5132 = DIRECTION ( 'NONE',  ( -1.000000000000000000, -0.000000000000000000, -0.000000000000000000 ) ) ;
#5133 = DIRECTION ( 'NONE',  ( -0.000000000000000000, -1.000000000000000000, -0.000000000000000000 ) ) ;
#5134 = CARTESIAN_POINT ( 'NONE',  ( 42.77500000054622831, 20.00000000000000355, 83.50966788445364841 ) ) ;
#5135 = AXIS2_PLACEMENT_3D ( 'NONE', #6026, #6779, #11543 ) ;
#5136 = FACE_OUTER_BOUND ( 'NONE', #8744, .T. ) ;
#5137 = ORIENTED_EDGE ( 'NONE', *, *, #8445, .T. ) ;
#5138 = CARTESIAN_POINT ( 'NONE',  ( -10.00000000000000355, 19.67057089699415684, -26.15339366124403853 ) ) ;
#5139 = EDGE_CURVE ( 'NONE', #4669, #6404, #578, .T. ) ;
#5140 = CONTEXT_DEPENDENT_SHAPE_REPRESENTATION ( #10880, #11551 ) ;
#5141 = CARTESIAN_POINT ( 'NONE',  ( 46.69999999999998153, 13.62011893735970958, 86.15790661882942914 ) ) ;
#5142 = CARTESIAN_POINT ( 'NONE',  ( 46.87500000054622262, 20.00000000000000355, 83.50966788445364841 ) ) ;
#5143 = CIRCLE ( 'NONE', #2304, 6.000000000000003553 ) ;
#5144 = CARTESIAN_POINT ( 'NONE',  ( 33.07500000054623257, 26.19570976099943849, 86.29171490190961435 ) ) ;
#5145 = EDGE_CURVE ( 'NONE', #6828, #378, #7287, .T. ) ;
#5146 = CARTESIAN_POINT ( 'NONE',  ( 22.47500000054622404, 13.07298590277314432, 88.54243821818161564 ) ) ;
#5147 = CARTESIAN_POINT ( 'NONE',  ( 49.99999999999998579, 0.000000000000000000, 82.99999999999995737 ) ) ;
#5148 = CYLINDRICAL_SURFACE ( 'NONE', #3431, 7.499999999999992895 ) ;
#5149 = CARTESIAN_POINT ( 'NONE',  ( 28.97500000054622760, 24.28113015263587471, 84.90069139318163138 ) ) ;
#5150 = VERTEX_POINT ( 'NONE', #6462 ) ;
#5151 = CARTESIAN_POINT ( 'NONE',  ( 22.95000000109246230, 26.37988106264029398, 86.15790661882942914 ) ) ;
#5152 = VERTEX_POINT ( 'NONE', #9139 ) ;
#5153 = VERTEX_POINT ( 'NONE', #8368 ) ;
#5154 = CARTESIAN_POINT ( 'NONE',  ( -6.999999999999999112, 69.50000000000000000, 146.8533255156881978 ) ) ;
#5155 = ORIENTED_EDGE ( 'NONE', *, *, #4592, .T. ) ;
#5156 = VECTOR ( 'NONE', #8975, 1000.000000000000000 ) ;
#5157 = DIRECTION ( 'NONE',  ( 1.000000000000000000, 0.000000000000000000, 0.000000000000000000 ) ) ;
#5158 = DIRECTION ( 'NONE',  ( 1.000000000000000000, 0.000000000000000000, 0.000000000000000000 ) ) ;
#5159 = CARTESIAN_POINT ( 'NONE',  ( 37.97500000054621694, 17.63344945572769973, 98.07665518445361386 ) ) ;
#5160 = CARTESIAN_POINT ( 'NONE',  ( -1.303021026755432743, 54.83843292061823149, -27.97152834316269576 ) ) ;
#5161 = CARTESIAN_POINT ( 'NONE',  ( -4.831992280633556014, 48.70433893284562998, -27.57995989914503809 ) ) ;
#5162 = CARTESIAN_POINT ( 'NONE',  ( 40.57500000054621836, 13.80429023900056684, 86.29171490190961435 ) ) ;
#5163 = CARTESIAN_POINT ( 'NONE',  ( 43.69999999999998863, 26.37988106264029398, 95.42841645007781892 ) ) ;
#5164 = CARTESIAN_POINT ( 'NONE',  ( 44.37500000054622973, 13.07298590277314432, 88.54243821818161564 ) ) ;
#5165 = ORIENTED_EDGE ( 'NONE', *, *, #6521, .T. ) ;
#5166 = VECTOR ( 'NONE', #3773, 1000.000000000000000 ) ;
#5167 = CARTESIAN_POINT ( 'NONE',  ( 24.85000000109246443, 24.40838939219355197, 84.72553407664153724 ) ) ;
#5168 = CARTESIAN_POINT ( 'NONE',  ( -9.869611566543289527, 18.35654797443324782, 22.96945393929722457 ) ) ;
#5169 = ORIENTED_EDGE ( 'NONE', *, *, #647, .T. ) ;
#5170 = CARTESIAN_POINT ( 'NONE',  ( -9.659644484749870585, 22.60756928696590862, -26.28120473514388777 ) ) ;
#5171 = ORIENTED_EDGE ( 'NONE', *, *, #11765, .T. ) ;
#5172 = FACE_OUTER_BOUND ( 'NONE', #8817, .T. ) ;
#5173 = CARTESIAN_POINT ( 'NONE',  ( 41.25000000109246656, 27.13292387221364876, 93.11078899226573924 ) ) ;
#5174 = CARTESIAN_POINT ( 'NONE',  ( 48.59999999999998721, 12.86707612778636012, 88.47553407664152303 ) ) ;
#5175 = AXIS2_PLACEMENT_3D ( 'NONE', #1126, #1062, #6945 ) ;
#5176 = CARTESIAN_POINT ( 'NONE',  ( 31.17500000054622689, 26.92701409722686634, 88.54243821818162985 ) ) ;
#5177 = CARTESIAN_POINT ( 'NONE',  ( 34.37500000054622973, 12.34168156654572535, 90.79316153445363113 ) ) ;
#5178 = DIRECTION ( 'NONE',  ( 0.000000000000000000, 1.000000000000000000, -0.000000000000000000 ) ) ;
#5179 = DIRECTION ( 'NONE',  ( -0.000000000000000000, -0.000000000000000000, 1.000000000000000000 ) ) ;
#5180 = CARTESIAN_POINT ( 'NONE',  ( 22.05000000109246372, 12.86707612778636012, 93.11078899226572503 ) ) ;
#5181 = VERTEX_POINT ( 'NONE', #11157 ) ;
#5182 = CARTESIAN_POINT ( 'NONE',  ( 43.95000000109245519, 13.62011893735971135, 95.42841645007781892 ) ) ;
#5183 = CARTESIAN_POINT ( 'NONE',  ( 2.571758291765529985E-15, 45.00000000000000711, 21.00000000000000000 ) ) ;
#5184 = EDGE_LOOP ( 'NONE', ( #2383, #11757, #4391 ) ) ;
#5185 = CARTESIAN_POINT ( 'NONE',  ( -28.50000000000001066, 84.49999999999998579, 146.8533255156881978 ) ) ;
#5186 = AXIS2_PLACEMENT_3D ( 'NONE', #1448, #371, #7396 ) ;
#5187 = EDGE_LOOP ( 'NONE', ( #5513, #6283 ) ) ;
#5188 = EDGE_CURVE ( 'NONE', #4064, #10, #10206, .T. ) ;
#5189 = CARTESIAN_POINT ( 'NONE',  ( -7.994063978020062912E-22, 10.00000000000000000, -21.00000000000000000 ) ) ;
#5190 = CARTESIAN_POINT ( 'NONE',  ( 6.000000000000000000, 5.839897972853064445, -8.673617379884035472E-15 ) ) ;
#5191 = TOROIDAL_SURFACE ( 'NONE', #10844, 6.599999999999998757, 0.5999999999999999778 ) ;
#5192 =( LENGTH_UNIT ( ) NAMED_UNIT ( * ) SI_UNIT ( .MILLI., .METRE. ) );
#5193 = CARTESIAN_POINT ( 'NONE',  ( -7.536850167683876833, 13.39586159374066021, 23.84162237519015548 ) ) ;
#5194 = CARTESIAN_POINT ( 'NONE',  ( 22.69999999999998153, 13.62011893735970958, 86.15790661882942914 ) ) ;
#5195 = CARTESIAN_POINT ( 'NONE',  ( -0.6585108229100932187, 45.03273675766970285, -24.99339394906690970 ) ) ;
#5196 = CARTESIAN_POINT ( 'NONE',  ( -4.336756015782423646, 52.50983733265497477, 20.54816100008359214 ) ) ;
#5197 = CARTESIAN_POINT ( 'NONE',  ( -0.6575419410981192536, 45.03270851040807088, 27.99410734628499853 ) ) ;
#5198 = CARTESIAN_POINT ( 'NONE',  ( 4.839481439987470601, 48.70147115714765107, 20.43486580129273733 ) ) ;
#5199 = ORIENTED_EDGE ( 'NONE', *, *, #418, .T. ) ;
#5200 = CARTESIAN_POINT ( 'NONE',  ( 6.000000000000000000, 2.919948986426538884, 5.057499999999996554 ) ) ;
#5201 = ITEM_DEFINED_TRANSFORMATION ( 'NONE', 'NONE', #683,  #9021 ) ;
#5202 = EDGE_CURVE ( 'NONE', #3966, #10690, #9956, .T. ) ;
#5203 = PLANE ( 'NONE',  #744 ) ;
#5204 = CARTESIAN_POINT ( 'NONE',  ( 47.17500000054622689, 26.19570976099943493, 86.29171490190961435 ) ) ;
#5205 = VECTOR ( 'NONE', #7851, 999.9999999999998863 ) ;
#5206 = CARTESIAN_POINT ( 'NONE',  ( 33.47500000054622404, 26.19570976099943849, 95.29460816699764791 ) ) ;
#5207 = CARTESIAN_POINT ( 'NONE',  ( 7.417742579741789299, 13.28838962888333342, 94.17527653944314636 ) ) ;
#5208 = CARTESIAN_POINT ( 'NONE',  ( 45.25000000109246656, 27.13292387221364876, 93.11078899226573924 ) ) ;
#5209 = CARTESIAN_POINT ( 'NONE',  ( 24.77500000054622831, 20.00000000000000355, 83.50966788445364841 ) ) ;
#5210 = ORIENTED_EDGE ( 'NONE', *, *, #7882, .F. ) ;
#5211 = CYLINDRICAL_SURFACE ( 'NONE', #11560, 7.499999999999992895 ) ;
#5212 = VERTEX_POINT ( 'NONE', #3600 ) ;
#5213 = ORIENTED_EDGE ( 'NONE', *, *, #4750, .T. ) ;
#5214 = DIRECTION ( 'NONE',  ( 0.000000000000000000, -0.5000000000000011102, -0.8660254037844379305 ) ) ;
#5215 = VERTEX_POINT ( 'NONE', #4558 ) ;
#5216 = AXIS2_PLACEMENT_3D ( 'NONE', #8293, #7331, #8044 ) ;
#5217 = DIRECTION ( 'NONE',  ( 0.000000000000000000, 0.000000000000000000, 1.000000000000000000 ) ) ;
#5218 = EDGE_CURVE ( 'NONE', #9799, #652, #5520, .T. ) ;
#5219 = CARTESIAN_POINT ( 'NONE',  ( 38.27500000054622831, 13.07298590277314254, 93.04388485072563242 ) ) ;
#5220 = CARTESIAN_POINT ( 'NONE',  ( 36.79999999999998295, 15.59161060780646046, 84.72553407664153724 ) ) ;
#5221 = DIRECTION ( 'NONE',  ( 0.000000000000000000, 0.000000000000000000, -1.000000000000000000 ) ) ;
#5222 = CARTESIAN_POINT ( 'NONE',  ( 40.27500000054622120, 13.07298590277314254, 93.04388485072563242 ) ) ;
#5223 = CARTESIAN_POINT ( 'NONE',  ( 37.69999999999998153, 26.37988106264029398, 95.42841645007781892 ) ) ;
#5224 = EDGE_CURVE ( 'NONE', #5153, #6070, #6705, .T. ) ;
#5225 = CARTESIAN_POINT ( 'NONE',  ( 43.77500000054622831, 20.00000000000000355, 98.07665518445361386 ) ) ;
#5226 = ORIENTED_EDGE ( 'NONE', *, *, #3945, .F. ) ;
#5227 = CARTESIAN_POINT ( 'NONE',  ( 27.05000000109246372, 27.13292387221364876, 88.47553407664153724 ) ) ;
#5228 = CARTESIAN_POINT ( 'NONE',  ( -8.488496443319393236, 14.70368316582932877, 23.51557330312556360 ) ) ;
#5229 = VERTEX_POINT ( 'NONE', #6519 ) ;
#5230 = CARTESIAN_POINT ( 'NONE',  ( -7.946804781952113927, 26.10495865974165142, 26.85128829824916252 ) ) ;
#5231 = ORIENTED_EDGE ( 'NONE', *, *, #9768, .F. ) ;
#5232 = EDGE_CURVE ( 'NONE', #2033, #8953, #6259, .T. ) ;
#5233 = CARTESIAN_POINT ( 'NONE',  ( 8.671847030689137981, 14.97805994402878227, 26.62596067411855572 ) ) ;
#5234 = CARTESIAN_POINT ( 'NONE',  ( 4.967195524026380760, 49.34122594216266577, -27.55596498020302576 ) ) ;
#5235 = LINE ( 'NONE', #9106, #8183 ) ;
#5236 = CARTESIAN_POINT ( 'NONE',  ( 30.07500000054622546, 13.80429023900056507, 95.29460816699764791 ) ) ;
#5237 = CARTESIAN_POINT ( 'NONE',  ( 22.57500000054622546, 13.80429023900056684, 86.29171490190961435 ) ) ;
#5238 = DIRECTION ( 'NONE',  ( 0.000000000000000000, 0.000000000000000000, 1.000000000000000000 ) ) ;
#5239 = DIRECTION ( 'NONE',  ( 0.000000000000000000, 0.000000000000000000, -1.000000000000000000 ) ) ;
#5240 = CIRCLE ( 'NONE', #1782, 6.999999999999964473 ) ;
#5241 = VERTEX_POINT ( 'NONE', #12422 ) ;
#5242 = CARTESIAN_POINT ( 'NONE',  ( 45.25000000109246656, 27.13292387221364876, 93.11078899226573924 ) ) ;
#5243 = ORIENTED_EDGE ( 'NONE', *, *, #8754, .T. ) ;
#5244 = CYLINDRICAL_SURFACE ( 'NONE', #1593, 25.00000000000000000 ) ;
#5245 = ADVANCED_FACE ( 'NONE', ( #12301 ), #185, .T. ) ;
#5246 = EDGE_LOOP ( 'NONE', ( #5973, #9831, #4348, #3181, #12140, #7642, #806, #11745, #3969, #8957, #6172, #2425, #3934, #5305, #12341, #10242 ) ) ;
#5247 = CARTESIAN_POINT ( 'NONE',  ( -9.868061339005878452, 18.34793401400264301, -22.97011835729309936 ) ) ;
#5248 = CARTESIAN_POINT ( 'NONE',  ( 0.000000000000000000, -5.839897972853063557, 6.938893903907228378E-15 ) ) ;
#5249 = VECTOR ( 'NONE', #6926, 1000.000000000000000 ) ;
#5250 = CARTESIAN_POINT ( 'NONE',  ( 29.69999999999998508, 26.37988106264029398, 95.42841645007781892 ) ) ;
#5251 = CARTESIAN_POINT ( 'NONE',  ( 4.741482771685880948, 51.61996731904482516, 24.54657867284130646 ) ) ;
#5252 = DIRECTION ( 'NONE',  ( 1.000000000000000000, 0.000000000000000000, 0.000000000000000000 ) ) ;
#5253 = EDGE_CURVE ( 'NONE', #5929, #9442, #3009, .T. ) ;
#5254 = CARTESIAN_POINT ( 'NONE',  ( 22.39999999999998437, 12.86707612778636012, 93.11078899226572503 ) ) ;
#5255 = DIRECTION ( 'NONE',  ( 1.000000000000000000, 0.000000000000000000, 0.000000000000000000 ) ) ;
#5256 = DIRECTION ( 'NONE',  ( -0.000000000000000000, -0.000000000000000000, 1.000000000000000000 ) ) ;
#5257 = DIRECTION ( 'NONE',  ( 0.000000000000000000, 0.8660254037844379305, -0.5000000000000012212 ) ) ;
#5258 = CIRCLE ( 'NONE', #1211, 17.50000000000000000 ) ;
#5259 = CARTESIAN_POINT ( 'NONE',  ( 34.99999999999999289, 20.00000000000000355, 189.9999999999999716 ) ) ;
#5260 = ORIENTED_EDGE ( 'NONE', *, *, #3507, .F. ) ;
#5261 = AXIS2_PLACEMENT_3D ( 'NONE', #5821, #4723, #986 ) ;
#5262 = CARTESIAN_POINT ( 'NONE',  ( -9.484541375895036097, 16.76356961828979308, -26.34605997290420376 ) ) ;
#5263 = CARTESIAN_POINT ( 'NONE',  ( 7.931072658818332677, 13.90045964729634420, -26.85413380561048413 ) ) ;
#5264 = CARTESIAN_POINT ( 'NONE',  ( 0.000000000000000000, 4.685197434473814759, -5.637851296924623057E-15 ) ) ;
#5265 = CARTESIAN_POINT ( 'NONE',  ( 42.87500000054622262, 20.00000000000000355, 83.50966788445364841 ) ) ;
#5266 = CARTESIAN_POINT ( 'NONE',  ( 25.27500000054622475, 27.65831843345427998, 90.79316153445363113 ) ) ;
#5267 = CARTESIAN_POINT ( 'NONE',  ( 9.684959410070431929, 17.49741726564071698, 83.71847969554855240 ) ) ;
#5268 = CARTESIAN_POINT ( 'NONE',  ( 45.35000000109246088, 26.37988106264029398, 95.42841645007781892 ) ) ;
#5269 = DIRECTION ( 'NONE',  ( -1.000000000000000000, -0.000000000000000000, -0.000000000000000000 ) ) ;
#5270 = CARTESIAN_POINT ( 'NONE',  ( 31.59999999999999076, 27.13292387221364876, 93.11078899226573924 ) ) ;
#5271 = CARTESIAN_POINT ( 'NONE',  ( 28.87500000054622262, 22.36655054427230382, 83.50966788445364841 ) ) ;
#5272 = ORIENTED_EDGE ( 'NONE', *, *, #4336, .F. ) ;
#5273 = EDGE_CURVE ( 'NONE', #1223, #2922, #8281, .T. ) ;
#5274 = DIRECTION ( 'NONE',  ( 0.000000000000000000, 0.000000000000000000, -1.000000000000000000 ) ) ;
#5275 = VERTEX_POINT ( 'NONE', #10386 ) ;
#5276 = FACE_OUTER_BOUND ( 'NONE', #10956, .T. ) ;
#5277 = VERTEX_POINT ( 'NONE', #4684 ) ;
#5278 =( LENGTH_UNIT ( ) NAMED_UNIT ( * ) SI_UNIT ( .MILLI., .METRE. ) );
#5279 = PRODUCT_DEFINITION ( 'UNKNOWN', '', #8187, #8027 ) ;
#5280 = ADVANCED_FACE ( 'NONE', ( #11350 ), #12528, .T. ) ;
#5281 = CARTESIAN_POINT ( 'NONE',  ( 33.27500000054622831, 26.92701409722686634, 88.54243821818162985 ) ) ;
#5282 = CARTESIAN_POINT ( 'NONE',  ( 49.99999999999998579, 18.00000000000000355, 69.99999999999998579 ) ) ;
#5283 = CARTESIAN_POINT ( 'NONE',  ( 48.77500000054622831, 20.00000000000000355, 83.50966788445364841 ) ) ;
#5284 = CARTESIAN_POINT ( 'NONE',  ( 32.77500000054622831, 17.63344945572770328, 83.50966788445364841 ) ) ;
#5285 = CARTESIAN_POINT ( 'NONE',  ( 36.99999999999999289, 20.00000000000000355, 83.29316153445364534 ) ) ;
#5286 = AXIS2_PLACEMENT_3D ( 'NONE', #2910, #8871, #1955 ) ;
#5287 = CARTESIAN_POINT ( 'NONE',  ( 45.57500000054622546, 24.28113015263587116, 96.68563167572563088 ) ) ;
#5288 = ORIENTED_EDGE ( 'NONE', *, *, #8089, .F. ) ;
#5289 = CARTESIAN_POINT ( 'NONE',  ( 21.75000000109246656, 17.56310227825320425, 98.29316153445363113 ) ) ;
#5290 = CARTESIAN_POINT ( 'NONE',  ( -4.838865259365938698, 48.69895664399926005, 24.52732495089485099 ) ) ;
#5291 = ORIENTED_EDGE ( 'NONE', *, *, #1344, .T. ) ;
#5292 = DIRECTION ( 'NONE',  ( 0.000000000000000000, 1.000000000000000000, 0.000000000000000000 ) ) ;
#5293 = VERTEX_POINT ( 'NONE', #3664 ) ;
#5294 = VECTOR ( 'NONE', #9720, 1000.000000000000000 ) ;
#5295 = CARTESIAN_POINT ( 'NONE',  ( 20.75000000109246301, 22.43689772174679575, 83.29316153445363113 ) ) ;
#5296 = PRODUCT_DEFINITION_SHAPE ( 'NONE', 'NONE',  #12548 ) ;
#5297 = EDGE_CURVE ( 'NONE', #7533, #6466, #9901, .T. ) ;
#5298 = CARTESIAN_POINT ( 'NONE',  ( -2.000000000000015543, 20.00000000000000355, 98.29316153445363113 ) ) ;
#5299 = CARTESIAN_POINT ( 'NONE',  ( 3.245314017740486159E-15, 70.00000000000000000, 25.00000000000000000 ) ) ;
#5300 = CARTESIAN_POINT ( 'NONE',  ( 24.07500000054622902, 13.80429023900056507, 95.29460816699764791 ) ) ;
#5301 = CARTESIAN_POINT ( 'NONE',  ( 23.67500000054622333, 24.28113015263587116, 96.68563167572563088 ) ) ;
#5302 = CARTESIAN_POINT ( 'NONE',  ( 10.00000000000000355, 20.00000000000000355, 26.15339366124404563 ) ) ;
#5303 = EDGE_CURVE ( 'NONE', #409, #9559, #752, .T. ) ;
#5304 = LINE ( 'NONE', #10241, #9088 ) ;
#5305 = ORIENTED_EDGE ( 'NONE', *, *, #3273, .F. ) ;
#5306 = VECTOR ( 'NONE', #11225, 1000.000000000000000 ) ;
#5307 = CARTESIAN_POINT ( 'NONE',  ( 43.15000000109247225, 27.88596668178699645, 90.79316153445363113 ) ) ;
#5308 = FILL_AREA_STYLE ('',( #4406 ) ) ;
#5309 = ORIENTED_EDGE ( 'NONE', *, *, #8252, .F. ) ;
#5310 = CARTESIAN_POINT ( 'NONE',  ( 0.000000000000000000, 2.342598717236900718, -4.057500000000001883 ) ) ;
#5311 = ORIENTED_EDGE ( 'NONE', *, *, #2346, .F. ) ;
#5312 = EDGE_CURVE ( 'NONE', #11275, #2279, #8492, .T. ) ;
#5313 = CARTESIAN_POINT ( 'NONE',  ( -8.972964902253410813, 15.53670184611763005, -23.33582545272828312 ) ) ;
#5314 = CARTESIAN_POINT ( 'NONE',  ( -4.149932937002940747, 29.10413268181202184, 24.65505180927770112 ) ) ;
#5315 = CARTESIAN_POINT ( 'NONE',  ( 20.97500000054622760, 24.28113015263587471, 84.90069139318163138 ) ) ;
#5316 = FILL_AREA_STYLE ('',( #2387 ) ) ;
#5317 = CARTESIAN_POINT ( 'NONE',  ( -8.488496443319393236, 14.70368316582932877, 23.51557330312556360 ) ) ;
#5318 = CARTESIAN_POINT ( 'NONE',  ( 0.000000000000000000, 139.9999999999999716, 0.000000000000000000 ) ) ;
#5319 = CARTESIAN_POINT ( 'NONE',  ( 0.6000000000000033085, 0.000000000000000000, 8.400000000000000355 ) ) ;
#5320 = CARTESIAN_POINT ( 'NONE',  ( -6.999999999999999112, 40.00000000000000000, 69.99999999999998579 ) ) ;
#5321 = CARTESIAN_POINT ( 'NONE',  ( 9.867555937047535863, 21.65500574101911724, 22.97033549711487410 ) ) ;
#5322 = CARTESIAN_POINT ( 'NONE',  ( 1.298746404259454534, 45.16883511797273343, 20.96039105888827692 ) ) ;
#5323 = ORIENTED_EDGE ( 'NONE', *, *, #2474, .T. ) ;
#5324 = CARTESIAN_POINT ( 'NONE',  ( -4.743460743378065558, 51.61424263853129446, 24.54619549801029166 ) ) ;
#5325 = CONTEXT_DEPENDENT_SHAPE_REPRESENTATION ( #10230, #4274 ) ;
#5326 = FACE_OUTER_BOUND ( 'NONE', #3475, .T. ) ;
#5327 = CARTESIAN_POINT ( 'NONE',  ( 28.19999999999998863, 15.59161060780645691, 96.86078899226572503 ) ) ;
#5328 = CARTESIAN_POINT ( 'NONE',  ( 47.07500000054622546, 24.28113015263587471, 84.90069139318163138 ) ) ;
#5329 = CARTESIAN_POINT ( 'NONE',  ( 23.97500000054623115, 15.71886984736413417, 96.68563167572563088 ) ) ;
#5330 = CARTESIAN_POINT ( 'NONE',  ( 8.486510062750307171, 14.70060591898896618, -23.51628241912814588 ) ) ;
#5331 = CARTESIAN_POINT ( 'NONE',  ( 45.05000000109246372, 27.13292387221364876, 88.47553407664153724 ) ) ;
#5332 = CIRCLE ( 'NONE', #1075, 9.499999999999994671 ) ;
#5333 = CARTESIAN_POINT ( 'NONE',  ( 39.99999999999998579, 20.00000000000000355, 98.29316153445363113 ) ) ;
#5334 = CYLINDRICAL_SURFACE ( 'NONE', #2822, 7.499999999999978684 ) ;
#5335 = ORIENTED_EDGE ( 'NONE', *, *, #9402, .F. ) ;
#5336 = CARTESIAN_POINT ( 'NONE',  ( -2.000000000000015543, 20.00000000000000355, 90.79316153445363113 ) ) ;
#5337 = VERTEX_POINT ( 'NONE', #1820 ) ;
#5338 = CARTESIAN_POINT ( 'NONE',  ( -2.000000000000015543, 20.00000000000000355, 90.79316153445363113 ) ) ;
#5339 = ORIENTED_EDGE ( 'NONE', *, *, #7376, .T. ) ;
#5340 = EDGE_CURVE ( 'NONE', #12462, #3844, #7669, .T. ) ;
#5341 = AXIS2_PLACEMENT_3D ( 'NONE', #9574, #755, #1949 ) ;
#5342 = CARTESIAN_POINT ( 'NONE',  ( 33.37500000054621552, 27.65831843345427998, 90.79316153445363113 ) ) ;
#5343 = CARTESIAN_POINT ( 'NONE',  ( 6.000000000000000000, 8.759846959279592227, -5.057500000000009877 ) ) ;
#5344 = CARTESIAN_POINT ( 'NONE',  ( 49.07500000054622546, 26.19570976099943849, 86.29171490190961435 ) ) ;
#5345 = CARTESIAN_POINT ( 'NONE',  ( 36.87500000054622262, 20.00000000000000355, 83.50966788445364841 ) ) ;
#5346 = CARTESIAN_POINT ( 'NONE',  ( 38.09999999999999432, 17.56310227825320425, 98.29316153445363113 ) ) ;
#5347 = CARTESIAN_POINT ( 'NONE',  ( 44.67500000054623399, 17.63344945572770328, 83.50966788445364841 ) ) ;
#5348 = ORIENTED_EDGE ( 'NONE', *, *, #9091, .F. ) ;
#5349 = CIRCLE ( 'NONE', #1499, 13.85889894354065710 ) ;
#5350 = CARTESIAN_POINT ( 'NONE',  ( 27.15000000109245804, 27.88596668178699645, 90.79316153445363113 ) ) ;
#5351 = CARTESIAN_POINT ( 'NONE',  ( -0.6591801397249409389, 45.03285316749953182, 24.99337097521990003 ) ) ;
#5352 = ORIENTED_EDGE ( 'NONE', *, *, #6989, .T. ) ;
#5353 = CARTESIAN_POINT ( 'NONE',  ( 0.000000000000000000, 50.00000000000000000, -28.00000000000000711 ) ) ;
#5354 = LINE ( 'NONE', #11471, #7688 ) ;
#5355 = VERTEX_POINT ( 'NONE', #12363 ) ;
#5356 = LINE ( 'NONE', #12080, #11642 ) ;
#5357 = CARTESIAN_POINT ( 'NONE',  ( 20.65000000109246514, 20.00000000000000355, 83.29316153445364534 ) ) ;
#5358 = CARTESIAN_POINT ( 'NONE',  ( 35.75000000109246656, 17.56310227825319004, 98.29316153445361692 ) ) ;
#5359 = CARTESIAN_POINT ( 'NONE',  ( 25.39999999999998792, 27.13292387221364876, 88.47553407664153724 ) ) ;
#5360 = EDGE_CURVE ( 'NONE', #9553, #10329, #12138, .T. ) ;
#5361 = ADVANCED_FACE ( 'NONE', ( #8614 ), #812, .F. ) ;
#5362 = CARTESIAN_POINT ( 'NONE',  ( 26.17500000054623044, 13.07298590277314254, 93.04388485072563242 ) ) ;
#5363 = CARTESIAN_POINT ( 'NONE',  ( 27.47500000054622404, 26.92701409722686634, 93.04388485072563242 ) ) ;
#5364 = VECTOR ( 'NONE', #2405, 999.9999999999998863 ) ;
#5365 = CARTESIAN_POINT ( 'NONE',  ( 0.6589055310361571216, 30.00000000000001776, 28.00000000000001421 ) ) ;
#5366 = CARTESIAN_POINT ( 'NONE',  ( 22.65000000109246514, 20.00000000000000355, 83.29316153445364534 ) ) ;
#5367 = ORIENTED_EDGE ( 'NONE', *, *, #12541, .T. ) ;
#5368 = EDGE_CURVE ( 'NONE', #2615, #850, #7675, .T. ) ;
#5369 = CARTESIAN_POINT ( 'NONE',  ( 45.65000000109247225, 20.00000000000000355, 98.29316153445363113 ) ) ;
#5370 = CARTESIAN_POINT ( 'NONE',  ( 4.840263798742708623, 51.29555919482307758, -24.52704763417973410 ) ) ;
#5371 = ORIENTED_EDGE ( 'NONE', *, *, #335, .T. ) ;
#5372 = ORIENTED_EDGE ( 'NONE', *, *, #3045, .T. ) ;
#5373 = CIRCLE ( 'NONE', #4142, 26.49999999999999645 ) ;
#5374 = CARTESIAN_POINT ( 'NONE',  ( -8.972964902253410813, 15.53670184611763005, -23.33582545272828312 ) ) ;
#5375 = CARTESIAN_POINT ( 'NONE',  ( 1.317448503741515342, 10.08163033484836113, -24.96744191981147409 ) ) ;
#5376 = ADVANCED_FACE ( 'NONE', ( #1013 ), #2210, .F. ) ;
#5377 = DIRECTION ( 'NONE',  ( 0.000000000000000000, 0.000000000000000000, 1.000000000000000000 ) ) ;
#5378 =( NAMED_UNIT ( * ) SI_UNIT ( $, .STERADIAN. ) SOLID_ANGLE_UNIT ( ) );
#5379 = DIRECTION ( 'NONE',  ( 0.000000000000000000, 0.000000000000000000, 1.000000000000000000 ) ) ;
#5380 = CYLINDRICAL_SURFACE ( 'NONE', #3218, 21.00000000000000000 ) ;
#5381 = VECTOR ( 'NONE', #7475, 999.9999999999998863 ) ;
#5382 = DIRECTION ( 'NONE',  ( 0.000000000000000000, -0.5000000000000012212, -0.8660254037844380415 ) ) ;
#5383 = EDGE_CURVE ( 'NONE', #2550, #5355, #2206, .T. ) ;
#5384 = CARTESIAN_POINT ( 'NONE',  ( 5.000000000000000000, 0.000000000000000000, 0.000000000000000000 ) ) ;
#5385 = CARTESIAN_POINT ( 'NONE',  ( 0.6586899486374204749, 30.00000000000001421, 25.00000000000000000 ) ) ;
#5386 = CARTESIAN_POINT ( 'NONE',  ( 47.15000000109245804, 27.88596668178699645, 90.79316153445363113 ) ) ;
#5387 = ORIENTED_EDGE ( 'NONE', *, *, #6227, .F. ) ;
#5388 = PLANE ( 'NONE',  #3980 ) ;
#5389 = VECTOR ( 'NONE', #5756, 1000.000000000000000 ) ;
#5390 = B_SPLINE_CURVE_WITH_KNOTS ( 'NONE', 3,
 ( #9298, #3209, #7071, #10948, #12088, #7257, #11132, #12275, #4654, #1733, #11381, #4593, #5737, #8404, #604, #12334, #4465, #8585, #2751, #2687 ),
 .UNSPECIFIED., .F., .F.,
 ( 4, 2, 2, 2, 2, 2, 2, 2, 2, 4 ),
 ( 0.007837842730401771429, 0.008817088216258357411, 0.009796333702114945127, 0.01028595644504323552, 0.01077557918797152590, 0.01175482467382810668, 0.01273407015968468919, 0.01371331564554126997, 0.01469256113139785075, 0.01567180661725443153 ),
 .UNSPECIFIED. ) ;
#5391 = CARTESIAN_POINT ( 'NONE',  ( 0.000000000000000000, 20.00000000000000355, 109.9999999999999858 ) ) ;
#5392 = CARTESIAN_POINT ( 'NONE',  ( 42.17500000054623399, 13.80429023900056507, 95.29460816699764791 ) ) ;
#5393 = CARTESIAN_POINT ( 'NONE',  ( 27.27500000054622475, 27.65831843345427998, 90.79316153445363113 ) ) ;
#5394 = CARTESIAN_POINT ( 'NONE',  ( 9.403487956461118458, 16.59018621808800020, 84.10865954674225975 ) ) ;
#5395 = CARTESIAN_POINT ( 'NONE',  ( 44.95000000109246230, 26.37988106264029398, 86.15790661882942914 ) ) ;
#5396 = DIRECTION ( 'NONE',  ( 1.000000000000000000, -0.000000000000000000, -0.000000000000000000 ) ) ;
#5397 = DIRECTION ( 'NONE',  ( 0.000000000000000000, 0.000000000000000000, -1.000000000000000000 ) ) ;
#5398 = ORIENTED_EDGE ( 'NONE', *, *, #9978, .F. ) ;
#5399 = CARTESIAN_POINT ( 'NONE',  ( -6.999999999999999112, 55.00000000000000000, 166.8533255156881694 ) ) ;
#5400 = ORIENTED_EDGE ( 'NONE', *, *, #1713, .T. ) ;
#5401 = DIRECTION ( 'NONE',  ( 0.000000000000000000, 0.000000000000000000, -1.000000000000000000 ) ) ;
#5402 = ORIENTED_EDGE ( 'NONE', *, *, #7457, .T. ) ;
#5403 = VECTOR ( 'NONE', #7727, 1000.000000000000000 ) ;
#5404 = CARTESIAN_POINT ( 'NONE',  ( 33.87500000054622262, 20.00000000000000355, 98.07665518445361386 ) ) ;
#5405 = CARTESIAN_POINT ( 'NONE',  ( -4.743784540849714126, 51.61351337007339168, -27.59551847071385566 ) ) ;
#5406 = CARTESIAN_POINT ( 'NONE',  ( 47.87500000054622973, 17.63344945572769973, 98.07665518445361386 ) ) ;
#5407 = CARTESIAN_POINT ( 'NONE',  ( 31.67500000054622333, 24.28113015263587116, 96.68563167572563088 ) ) ;
#5408 = CARTESIAN_POINT ( 'NONE',  ( 33.39999999999998437, 27.13292387221364876, 88.47553407664153724 ) ) ;
#5409 = CARTESIAN_POINT ( 'NONE',  ( -8.119709436525981872, 25.84588397371641122, 19.36772275760405648 ) ) ;
#5410 = EDGE_CURVE ( 'NONE', #2987, #3859, #9101, .T. ) ;
#5411 = CARTESIAN_POINT ( 'NONE',  ( 41.87500000054622262, 17.63344945572769973, 98.07665518445361386 ) ) ;
#5412 = VERTEX_POINT ( 'NONE', #3915 ) ;
#5413 = CARTESIAN_POINT ( 'NONE',  ( 25.15000000109246159, 27.88596668178699645, 90.79316153445363113 ) ) ;
#5414 = CARTESIAN_POINT ( 'NONE',  ( -1.300905012451813336, 45.16112489716824996, 24.96819491493427634 ) ) ;
#5415=STYLED_ITEM('',(#12591),#10384);
#5416 = VERTEX_POINT ( 'NONE', #7855 ) ;
#5417 = CARTESIAN_POINT ( 'NONE',  ( -9.935474497414313433, 21.31256710255370379, -26.17833964914451172 ) ) ;
#5418 = ORIENTED_EDGE ( 'NONE', *, *, #2500, .T. ) ;
#5419 = DIRECTION ( 'NONE',  ( 1.000000000000000000, -0.000000000000000000, -0.000000000000000000 ) ) ;
#5420 = DIRECTION ( 'NONE',  ( -0.000000000000000000, -0.000000000000000000, 1.000000000000000000 ) ) ;
#5421 = CARTESIAN_POINT ( 'NONE',  ( 36.25000000109246656, 12.86707612778636012, 88.47553407664152303 ) ) ;
#5422 = CARTESIAN_POINT ( 'NONE',  ( 32.35000000109246088, 13.62011893735970958, 86.15790661882942914 ) ) ;
#5423 = AXIS2_PLACEMENT_3D ( 'NONE', #11764, #10875, #6056 ) ;
#5424 = CARTESIAN_POINT ( 'NONE',  ( 26.27500000054622475, 12.34168156654572535, 90.79316153445363113 ) ) ;
#5425 = CARTESIAN_POINT ( 'NONE',  ( 25.87500000054622618, 20.00000000000000355, 98.07665518445361386 ) ) ;
#5426 = DIRECTION ( 'NONE',  ( -1.000000000000000000, 0.000000000000000000, 0.000000000000000000 ) ) ;
#5427 = CARTESIAN_POINT ( 'NONE',  ( 0.000000000000000000, 18.00000000000000355, 169.9999999999999716 ) ) ;
#5428 = VERTEX_POINT ( 'NONE', #2070 ) ;
#5429 = CARTESIAN_POINT ( 'NONE',  ( 43.85000000109246798, 15.59161060780645691, 96.86078899226572503 ) ) ;
#5430 = SURFACE_STYLE_FILL_AREA ( #9176 ) ;
#5431 = VERTEX_POINT ( 'NONE', #11850 ) ;
#5432 = CARTESIAN_POINT ( 'NONE',  ( 29.75000000109246301, 17.56310227825320425, 98.29316153445363113 ) ) ;
#5433 = EDGE_CURVE ( 'NONE', #5434, #10300, #6836, .T. ) ;
#5434 = VERTEX_POINT ( 'NONE', #5130 ) ;
#5435 = VECTOR ( 'NONE', #7316, 1000.000000000000000 ) ;
#5436 = CARTESIAN_POINT ( 'NONE',  ( 2.559760333650129958E-15, 55.00000000000000000, 21.00000000000000000 ) ) ;
#5437 = CARTESIAN_POINT ( 'NONE',  ( -9.673352204464322313, 22.61971715202064104, 23.05311956053869338 ) ) ;
#5438 = PRODUCT_DEFINITION ( 'UNKNOWN', '', #4740, #3203 ) ;
#5439 = CARTESIAN_POINT ( 'NONE',  ( 28.99999999999998934, 20.00000000000000355, 83.29316153445364534 ) ) ;
#5440 = EDGE_CURVE ( 'NONE', #1159, #8255, #11724, .T. ) ;
#5441 = AXIS2_PLACEMENT_3D ( 'NONE', #10545, #1855, #9362 ) ;
#5442 = CARTESIAN_POINT ( 'NONE',  ( 38.25000000109246656, 12.86707612778636012, 88.47553407664152303 ) ) ;
#5443 = CARTESIAN_POINT ( 'NONE',  ( 0.000000000000000000, 0.000000000000000000, 0.000000000000000000 ) ) ;
#5444 = CARTESIAN_POINT ( 'NONE',  ( 42.79999999999999005, 15.59161060780646046, 84.72553407664153724 ) ) ;
#5445 = DIRECTION ( 'NONE',  ( 1.000000000000000000, 0.000000000000000000, 0.000000000000000000 ) ) ;
#5446 = CARTESIAN_POINT ( 'NONE',  ( 5.000000000000000000, 2.342598717236900718, -4.057500000000001883 ) ) ;
#5447 = CARTESIAN_POINT ( 'NONE',  ( -0.6582364880112170358, 54.96720335004231828, 24.99338302292539638 ) ) ;
#5448 = ORIENTED_EDGE ( 'NONE', *, *, #8971, .T. ) ;
#5449 =( BOUNDED_CURVE ( )  B_SPLINE_CURVE ( 2, ( #6329, #10200, #1510, #8302, #3474, #7339, #3846, #8607, #3197, #10937, #2898 ),
 .UNSPECIFIED., .F., .F. ) 
 B_SPLINE_CURVE_WITH_KNOTS ( ( 3, 2, 2, 2, 2, 3 ),
 ( 0.8666666666666666963, 0.8733333333333332948, 0.8800000000000000044, 0.8866666666666667140, 0.8933333333333333126, 0.9000000000000000222 ),
 .UNSPECIFIED. ) 
 CURVE ( )  GEOMETRIC_REPRESENTATION_ITEM ( )  RATIONAL_B_SPLINE_CURVE ( ( 1.000000000000000000, 0.9510565162951535312, 1.000000000000000000, 0.9510565162951535312, 1.000000000000000000, 0.9510565162951535312, 1.000000000000000000, 0.9510565162951535312, 1.000000000000000000, 0.9510565162951535312, 1.000000000000000000 ) ) 
 REPRESENTATION_ITEM ( '' )  );
#5450 = AXIS2_PLACEMENT_3D ( 'NONE', #3125, #9670, #6803 ) ;
#5451 = AXIS2_PLACEMENT_3D ( 'NONE', #6681, #2093, #11803 ) ;
#5452 = B_SPLINE_CURVE_WITH_KNOTS ( 'NONE', 3,
 ( #5436, #12284, #2567, #5619, #11326, #731, #6383, #8472, #4355, #2635, #10190, #9430, #12342, #10248, #11387, #2696, #8227, #3398 ),
 .UNSPECIFIED., .F., .F.,
 ( 4, 2, 2, 2, 2, 2, 2, 2, 4 ),
 ( 0.02353265389067876051, 0.02451271468972987533, 0.02549277548878099361, 0.02647283628783211190, 0.02745289708688322672, 0.02843295788593434500, 0.02941301868498545982, 0.03039307948403657811, 0.03137314028308769293 ),
 .UNSPECIFIED. ) ;
#5453 = CARTESIAN_POINT ( 'NONE',  ( 3.303926766530076442, 46.23304915065238418, 24.78181020466353601 ) ) ;
#5454 = EDGE_CURVE ( 'NONE', #6993, #4807, #6858, .T. ) ;
#5455 = CARTESIAN_POINT ( 'NONE',  ( 4.838449599032471404, 51.30291823734444989, 24.52740775798701378 ) ) ;
#5456 = CARTESIAN_POINT ( 'NONE',  ( 39.37500000054622262, 27.65831843345427998, 90.79316153445363113 ) ) ;
#5457 = CARTESIAN_POINT ( 'NONE',  ( 28.27500000054622475, 12.34168156654572357, 90.79316153445363113 ) ) ;
#5458 = VECTOR ( 'NONE', #3993, 1000.000000000000000 ) ;
#5459 = CARTESIAN_POINT ( 'NONE',  ( 6.687975528478859566, 12.56545023609454681, 91.81450773486812977 ) ) ;
#5460 = CARTESIAN_POINT ( 'NONE',  ( 5.000000000000000000, 50.00000000000000000, 24.49489742783178059 ) ) ;
#5461 = APPLICATION_CONTEXT ( 'automotive_design' ) ;
#5462 = CARTESIAN_POINT ( 'NONE',  ( 33.99999999999998579, 20.00000000000000355, 98.29316153445363113 ) ) ;
#5463 = DIRECTION ( 'NONE',  ( 1.000000000000000000, -0.000000000000000000, -0.000000000000000000 ) ) ;
#5464 = ADVANCED_FACE ( 'NONE', ( #10635 ), #5890, .F. ) ;
#5465 = VERTEX_POINT ( 'NONE', #4172 ) ;
#5466 = CARTESIAN_POINT ( 'NONE',  ( 6.000000000000000000, 0.000000000000000000, 0.000000000000000000 ) ) ;
#5467 = VERTEX_POINT ( 'NONE', #5827 ) ;
#5468 = DIRECTION ( 'NONE',  ( -1.000000000000000000, -0.000000000000000000, -0.000000000000000000 ) ) ;
#5469 = DIRECTION ( 'NONE',  ( 0.000000000000000000, 0.9242245927363030855, 0.3818493186865927203 ) ) ;
#5470 = VECTOR ( 'NONE', #7607, 1000.000000000000000 ) ;
#5471 = AXIS2_PLACEMENT_3D ( 'NONE', #8907, #2253, #3261 ) ;
#5472 = CARTESIAN_POINT ( 'NONE',  ( 34.97500000054622404, 22.36655054427230382, 83.50966788445364841 ) ) ;
#5473 = DIRECTION ( 'NONE',  ( 0.000000000000000000, 0.000000000000000000, 1.000000000000000000 ) ) ;
#5474 = CARTESIAN_POINT ( 'NONE',  ( 46.87500000054622262, 22.36655054427230382, 83.50966788445364841 ) ) ;
#5475 = CARTESIAN_POINT ( 'NONE',  ( 35.17500000054621268, 26.19570976099943493, 86.29171490190961435 ) ) ;
#5476 = CARTESIAN_POINT ( 'NONE',  ( 36.09999999999999432, 17.56310227825320425, 98.29316153445363113 ) ) ;
#5477 = CARTESIAN_POINT ( 'NONE',  ( -4.453030037920870932, 28.95979054136405395, 20.52457521359105996 ) ) ;
#5478 = CARTESIAN_POINT ( 'NONE',  ( 37.67500000054623399, 22.36655054427230027, 98.07665518445361386 ) ) ;
#5479 = ORIENTED_EDGE ( 'NONE', *, *, #8808, .T. ) ;
#5480 = CARTESIAN_POINT ( 'NONE',  ( 47.67500000054622689, 22.36655054427230027, 98.07665518445361386 ) ) ;
#5481 = LINE ( 'NONE', #6597, #9943 ) ;
#5482 = ORIENTED_EDGE ( 'NONE', *, *, #471, .F. ) ;
#5483 = CARTESIAN_POINT ( 'NONE',  ( -7.530077746149031803, 26.61198218432872764, -26.97262320105976485 ) ) ;
#5484 = ORIENTED_EDGE ( 'NONE', *, *, #4134, .F. ) ;
#5485 = FACE_OUTER_BOUND ( 'NONE', #4954, .T. ) ;
#5486 = DIRECTION ( 'NONE',  ( -1.000000000000000000, 0.000000000000000000, -0.000000000000000000 ) ) ;
#5487 = EDGE_CURVE ( 'NONE', #513, #574, #7141, .T. ) ;
#5488 = VECTOR ( 'NONE', #1295, 1000.000000000000114 ) ;
#5489 = DIRECTION ( 'NONE',  ( 0.000000000000000000, -0.5000000000000012212, -0.8660254037844380415 ) ) ;
#5490 = CARTESIAN_POINT ( 'NONE',  ( 25.97500000054622760, 15.71886984736413417, 96.68563167572563088 ) ) ;
#5491 = CARTESIAN_POINT ( 'NONE',  ( 23.97500000054622049, 17.63344945572769973, 98.07665518445361386 ) ) ;
#5492 = DIRECTION ( 'NONE',  ( -1.000000000000000000, -0.000000000000000000, -0.000000000000000000 ) ) ;
#5493 = CARTESIAN_POINT ( 'NONE',  ( 39.35000000109246088, 26.37988106264029398, 95.42841645007781892 ) ) ;
#5494 = ORIENTED_EDGE ( 'NONE', *, *, #7004, .F. ) ;
#5495 = CARTESIAN_POINT ( 'NONE',  ( 40.75000000109245946, 22.43689772174679575, 83.29316153445363113 ) ) ;
#5496 = SURFACE_SIDE_STYLE ('',( #1859 ) ) ;
#5497 = ORIENTED_EDGE ( 'NONE', *, *, #9171, .F. ) ;
#5498 = LINE ( 'NONE', #1495, #9311 ) ;
#5499 = AXIS2_PLACEMENT_3D ( 'NONE', #6392, #4610, #5572 ) ;
#5500 = ORIENTED_EDGE ( 'NONE', *, *, #3281, .F. ) ;
#5501 = CARTESIAN_POINT ( 'NONE',  ( -9.917336477930691174, 18.67442475474294028, -22.94880690262607459 ) ) ;
#5502 = CARTESIAN_POINT ( 'NONE',  ( 9.867746314566257837, 18.34543089117788028, -18.53734326927642684 ) ) ;
#5503 = EDGE_CURVE ( 'NONE', #2004, #589, #181, .T. ) ;
#5504 = DIRECTION ( 'NONE',  ( 0.000000000000000000, 0.000000000000000000, -1.000000000000000000 ) ) ;
#5505 = EDGE_CURVE ( 'NONE', #11823, #6070, #6014, .T. ) ;
#5506 = FACE_OUTER_BOUND ( 'NONE', #141, .T. ) ;
#5507 = CARTESIAN_POINT ( 'NONE',  ( -5.000000000000000000, 50.00000000000000000, 20.39607805437114152 ) ) ;
#5508 = CARTESIAN_POINT ( 'NONE',  ( 42.89999999999998437, 17.56310227825321491, 83.29316153445364534 ) ) ;
#5509 = DIRECTION ( 'NONE',  ( -1.000000000000000000, -0.000000000000000000, -0.000000000000000000 ) ) ;
#5510 = CARTESIAN_POINT ( 'NONE',  ( 29.67500000054623044, 22.36655054427230027, 98.07665518445361386 ) ) ;
#5511 = CARTESIAN_POINT ( 'NONE',  ( -50.00000000000001421, 20.00000000000000000, 137.5000000000000000 ) ) ;
#5512 = CARTESIAN_POINT ( 'NONE',  ( -5.000000000000000000, 50.00000000000000000, 24.49489742783178414 ) ) ;
#5513 = ORIENTED_EDGE ( 'NONE', *, *, #12033, .T. ) ;
#5514 = CARTESIAN_POINT ( 'NONE',  ( 0.000000000000000000, -2.919948986426538440, -5.057499999999997442 ) ) ;
#5515 = CARTESIAN_POINT ( 'NONE',  ( 0.000000000000000000, 20.00000000000000355, 109.9999999999999858 ) ) ;
#5516 = CARTESIAN_POINT ( 'NONE',  ( 37.27500000054622831, 27.65831843345427998, 90.79316153445363113 ) ) ;
#5517 = CARTESIAN_POINT ( 'NONE',  ( 40.07500000054623257, 15.71886984736413417, 96.68563167572563088 ) ) ;
#5518 = ADVANCED_FACE ( 'NONE', ( #7334 ), #6325, .F. ) ;
#5519 = CARTESIAN_POINT ( 'NONE',  ( 27.47500000054622049, 26.19570976099943849, 95.29460816699764791 ) ) ;
#5520 = LINE ( 'NONE', #8555, #8890 ) ;
#5521 = DIRECTION ( 'NONE',  ( 0.000000000000000000, 0.000000000000000000, -1.000000000000000000 ) ) ;
#5522 = CARTESIAN_POINT ( 'NONE',  ( 33.89999999999998437, 22.43689772174679575, 98.29316153445363113 ) ) ;
#5523 = CARTESIAN_POINT ( 'NONE',  ( 45.00000000000000000, 20.00000000000000711, 187.9999999999999716 ) ) ;
#5524 =( BOUNDED_CURVE ( )  B_SPLINE_CURVE ( 3, ( #5810, #11770, #1060, #6941 ),
 .UNSPECIFIED., .F., .F. ) 
 B_SPLINE_CURVE_WITH_KNOTS ( ( 4, 4 ),
 ( 4.712388980384689674, 6.013252511346182771 ),
 .UNSPECIFIED. ) 
 CURVE ( )  GEOMETRIC_REPRESENTATION_ITEM ( )  RATIONAL_B_SPLINE_CURVE ( ( 1.000000000000000000, 0.8638816171694809753, 0.8638816171694809753, 1.000000000000000000 ) ) 
 REPRESENTATION_ITEM ( '' )  );
#5525 = VERTEX_POINT ( 'NONE', #12164 ) ;
#5526 = EDGE_CURVE ( 'NONE', #11275, #1359, #4482, .T. ) ;
#5527 = FACE_BOUND ( 'NONE', #5645, .T. ) ;
#5528 = ORIENTED_EDGE ( 'NONE', *, *, #6826, .F. ) ;
#5529 = CARTESIAN_POINT ( 'NONE',  ( 27.50000000000000355, 12.50000000000001066, 145.0000000000000000 ) ) ;
#5530 = APPLICATION_PROTOCOL_DEFINITION ( 'draft international standard', 'automotive_design', 1998, #3666 ) ;
#5531 = EDGE_CURVE ( 'NONE', #6723, #6737, #6140, .T. ) ;
#5532 = CARTESIAN_POINT ( 'NONE',  ( 34.17500000054622689, 13.80429023900056507, 95.29460816699764791 ) ) ;
#5533 = DIRECTION ( 'NONE',  ( 0.000000000000000000, 0.000000000000000000, 1.000000000000000000 ) ) ;
#5534 = CARTESIAN_POINT ( 'NONE',  ( 45.07500000054621836, 26.19570976099943849, 86.29171490190961435 ) ) ;
#5535 = CARTESIAN_POINT ( 'NONE',  ( 36.27500000054622120, 13.07298590277314254, 93.04388485072563242 ) ) ;
#5536 = CARTESIAN_POINT ( 'NONE',  ( 32.79999999999999005, 15.59161060780646046, 84.72553407664153724 ) ) ;
#5537 = CARTESIAN_POINT ( 'NONE',  ( 8.664233696039474353, 25.03468766560890302, 23.45371044974007901 ) ) ;
#5538 = CARTESIAN_POINT ( 'NONE',  ( 39.87500000054622262, 17.63344945572769973, 98.07665518445361386 ) ) ;
#5539 = ORIENTED_EDGE ( 'NONE', *, *, #3707, .T. ) ;
#5540 = CARTESIAN_POINT ( 'NONE',  ( 49.27500000054623541, 27.65831843345427998, 90.79316153445363113 ) ) ;
#5541 = DIRECTION ( 'NONE',  ( 0.000000000000000000, 1.000000000000000000, 0.000000000000000000 ) ) ;
#5542 = ORIENTED_EDGE ( 'NONE', *, *, #3045, .F. ) ;
#5543 = CARTESIAN_POINT ( 'NONE',  ( -3.709758735690515970E-18, 30.00000000000001066, -25.00000000000000000 ) ) ;
#5544 = VERTEX_POINT ( 'NONE', #7273 ) ;
#5545 = AXIS2_PLACEMENT_3D ( 'NONE', #1463, #511, #4373 ) ;
#5546 = CARTESIAN_POINT ( 'NONE',  ( 2.294321452706637121, 29.73876067080973229, -24.89658462890612967 ) ) ;
#5547 = LINE ( 'NONE', #4335, #2824 ) ;
#5548 = DIRECTION ( 'NONE',  ( 1.000000000000000000, 0.000000000000000000, 0.000000000000000000 ) ) ;
#5549 = CARTESIAN_POINT ( 'NONE',  ( -2.000000000000015543, 20.00000000000000355, 90.79316153445363113 ) ) ;
#5550 = CARTESIAN_POINT ( 'NONE',  ( 25.87500000054622262, 17.63344945572769973, 98.07665518445361386 ) ) ;
#5551 = CARTESIAN_POINT ( 'NONE',  ( 49.39999999999998437, 27.13292387221364876, 88.47553407664153724 ) ) ;
#5552 = CARTESIAN_POINT ( 'NONE',  ( -28.50000000000001066, 77.00000000000000000, 166.8533255156881694 ) ) ;
#5553 = LINE ( 'NONE', #10295, #4414 ) ;
#5554 = ORIENTED_EDGE ( 'NONE', *, *, #6489, .T. ) ;
#5555 = CARTESIAN_POINT ( 'NONE',  ( 36.65000000109245804, 20.00000000000000355, 83.29316153445364534 ) ) ;
#5556 = SURFACE_STYLE_USAGE ( .BOTH. , #5496 ) ;
#5557 = VERTEX_POINT ( 'NONE', #4296 ) ;
#5558 = CYLINDRICAL_SURFACE ( 'NONE', #10041, 7.500000000000000000 ) ;
#5559 = EDGE_LOOP ( 'NONE', ( #4379, #9456, #10810 ) ) ;
#5560 = CARTESIAN_POINT ( 'NONE',  ( -9.481501190889247255, 16.75403870714897536, -23.13387092261990574 ) ) ;
#5561 = VECTOR ( 'NONE', #9433, 1000.000000000000000 ) ;
#5562 = CARTESIAN_POINT ( 'NONE',  ( -7.994063978020062912E-22, 10.00000000000000000, -21.00000000000000000 ) ) ;
#5563 = AXIS2_PLACEMENT_3D ( 'NONE', #358, #5426, #602 ) ;
#5564 = CARTESIAN_POINT ( 'NONE',  ( 0.000000000000000000, 0.000000000000000000, 0.000000000000000000 ) ) ;
#5565 = CARTESIAN_POINT ( 'NONE',  ( -2.511626000443172746, 45.66440847798708091, 20.85104232884582487 ) ) ;
#5566 = FACE_OUTER_BOUND ( 'NONE', #4158, .T. ) ;
#5567 = DIRECTION ( 'NONE',  ( -1.000000000000000000, -0.000000000000000000, -0.000000000000000000 ) ) ;
#5568 = CARTESIAN_POINT ( 'NONE',  ( 20.57500000054622902, 15.71886984736413773, 84.90069139318163138 ) ) ;
#5569 = ADVANCED_FACE ( 'NONE', ( #3469, #495 ), #3285, .T. ) ;
#5570 = CARTESIAN_POINT ( 'NONE',  ( 5.021458388981292487, 28.65403010179421983, 24.49227020900855933 ) ) ;
#5571 = AXIS2_PLACEMENT_3D ( 'NONE', #12425, #9514, #4815 ) ;
#5572 = DIRECTION ( 'NONE',  ( 1.000000000000000000, 0.000000000000000000, -0.000000000000000000 ) ) ;
#5573 = VERTEX_POINT ( 'NONE', #8172 ) ;
#5574 = PLANE ( 'NONE',  #7424 ) ;
#5575 = CARTESIAN_POINT ( 'NONE',  ( -50.00000000000001421, 18.00000000000000355, 152.2284161474004520 ) ) ;
#5576 = CARTESIAN_POINT ( 'NONE',  ( 37.17500000054620557, 26.19570976099943493, 86.29171490190961435 ) ) ;
#5577 = AXIS2_PLACEMENT_3D ( 'NONE', #8139, #12005, #4966 ) ;
#5578 = CARTESIAN_POINT ( 'NONE',  ( 23.17500000054622689, 26.92701409722686634, 88.54243821818162985 ) ) ;
#5579 = AXIS2_PLACEMENT_3D ( 'NONE', #1249, #7970, #5120 ) ;
#5580 = DIRECTION ( 'NONE',  ( -1.000000000000000000, 0.000000000000000000, 0.000000000000000000 ) ) ;
#5581 = DIRECTION ( 'NONE',  ( 1.000000000000000000, 0.000000000000000000, 0.000000000000000000 ) ) ;
#5582 = DIRECTION ( 'NONE',  ( 0.000000000000000000, 0.000000000000000000, 1.000000000000000000 ) ) ;
#5583 = DIRECTION ( 'NONE',  ( -1.000000000000000000, -0.000000000000000000, -0.000000000000000000 ) ) ;
#5584 = CARTESIAN_POINT ( 'NONE',  ( -10.00000000000000355, 20.00000000000000355, -28.00000000000000711 ) ) ;
#5585 = ORIENTED_EDGE ( 'NONE', *, *, #729, .F. ) ;
#5586 = FACE_OUTER_BOUND ( 'NONE', #8684, .T. ) ;
#5587 = ADVANCED_FACE ( 'NONE', ( #11204 ), #5380, .F. ) ;
#5588 = APPLICATION_PROTOCOL_DEFINITION ( 'draft international standard', 'automotive_design', 1998, #1566 ) ;
#5589 = AXIS2_PLACEMENT_3D ( 'NONE', #10686, #2127, #4991 ) ;
#5590 = CARTESIAN_POINT ( 'NONE',  ( 25.37500000054622618, 27.65831843345427998, 90.79316153445363113 ) ) ;
#5591 = CARTESIAN_POINT ( 'NONE',  ( 10.00000000000000355, 20.00000000000000355, -18.46618531261938401 ) ) ;
#5592 = CARTESIAN_POINT ( 'NONE',  ( 42.77500000054622831, 20.00000000000000355, 83.50966788445364841 ) ) ;
#5593 = CARTESIAN_POINT ( 'NONE',  ( 30.27500000054622475, 13.07298590277314254, 93.04388485072563242 ) ) ;
#5594 = CARTESIAN_POINT ( 'NONE',  ( 31.79999999999998650, 24.40838939219354842, 96.86078899226572503 ) ) ;
#5595 = SURFACE_SIDE_STYLE ('',( #7556 ) ) ;
#5596 = CARTESIAN_POINT ( 'NONE',  ( 41.57500000054623257, 24.28113015263587116, 96.68563167572563088 ) ) ;
#5597 = ORIENTED_EDGE ( 'NONE', *, *, #5994, .T. ) ;
#5598 = CARTESIAN_POINT ( 'NONE',  ( 48.27500000054622120, 12.34168156654572535, 90.79316153445363113 ) ) ;
#5599 = DIRECTION ( 'NONE',  ( -0.7071067811865452413, 8.659560562354961208E-17, -0.7071067811865497932 ) ) ;
#5600 = ORIENTED_EDGE ( 'NONE', *, *, #7210, .F. ) ;
#5601 = EDGE_CURVE ( 'NONE', #10486, #2485, #8356, .T. ) ;
#5602 = FACE_OUTER_BOUND ( 'NONE', #8839, .T. ) ;
#5603 = ORIENTED_EDGE ( 'NONE', *, *, #11101, .F. ) ;
#5604 = CARTESIAN_POINT ( 'NONE',  ( 42.15000000109246514, 12.11403331821300533, 90.79316153445363113 ) ) ;
#5605 = FACE_OUTER_BOUND ( 'NONE', #4160, .T. ) ;
#5606 = CARTESIAN_POINT ( 'NONE',  ( 47.07500000054622546, 24.28113015263587471, 84.90069139318163138 ) ) ;
#5607 = DIRECTION ( 'NONE',  ( 0.000000000000000000, -0.4999999999999985012, 0.8660254037844394848 ) ) ;
#5608 = EDGE_CURVE ( 'NONE', #2364, #7013, #9123, .T. ) ;
#5609 = CARTESIAN_POINT ( 'NONE',  ( 43.67500000054621978, 24.28113015263587116, 96.68563167572563088 ) ) ;
#5610 = CARTESIAN_POINT ( 'NONE',  ( 46.19999999999998863, 15.59161060780645691, 96.86078899226572503 ) ) ;
#5611 = CARTESIAN_POINT ( 'NONE',  ( 0.000000000000000000, -4.685197434473812983, 6.938893903907228378E-15 ) ) ;
#5612 = DIRECTION ( 'NONE',  ( 0.000000000000000000, 1.000000000000000000, -1.039664082171044875E-15 ) ) ;
#5613 = ORIENTED_EDGE ( 'NONE', *, *, #2508, .F. ) ;
#5614 = CARTESIAN_POINT ( 'NONE',  ( 38.35000000109246798, 13.62011893735971135, 86.15790661882942914 ) ) ;
#5615 = CARTESIAN_POINT ( 'NONE',  ( 8.975091145622032585, 15.54177410167867990, 23.33498156074052687 ) ) ;
#5616 = VERTEX_POINT ( 'NONE', #4360 ) ;
#5617 = ADVANCED_FACE ( 'NONE', ( #12223 ), #12040, .T. ) ;
#5618 = EDGE_LOOP ( 'NONE', ( #11934, #1049, #4639, #4047, #4517, #7195, #515, #4913, #9332, #9986, #4179, #10997, #11224, #9748, #4457, #4788, #2862, #8223, #1919, #5243, #4122, #301, #5323, #2356, #8550, #5199, #4851, #4312, #12445, #12001, #423, #201, #11164 ) ) ;
#5619 = CARTESIAN_POINT ( 'NONE',  ( 1.296662627741595797, 54.84000786826194229, 20.96239067773004905 ) ) ;
#5620 = VECTOR ( 'NONE', #11403, 1000.000000000000000 ) ;
#5621 = CARTESIAN_POINT ( 'NONE',  ( 30.95000000109246940, 26.37988106264029398, 86.15790661882942914 ) ) ;
#5622 = APPLICATION_CONTEXT ( 'automotive_design' ) ;
#5623 = CARTESIAN_POINT ( 'NONE',  ( -9.103371648737914157, 24.15160165414906857, 23.28405058525132176 ) ) ;
#5624 = DIRECTION ( 'NONE',  ( 0.000000000000000000, 0.000000000000000000, 1.000000000000000000 ) ) ;
#5625 = DIRECTION ( 'NONE',  ( 0.000000000000000000, 0.000000000000000000, -1.000000000000000000 ) ) ;
#5626 = CARTESIAN_POINT ( 'NONE',  ( 5.000000000000000000, 5.258101095580057891E-15, 4.057500000000001883 ) ) ;
#5627 = CARTESIAN_POINT ( 'NONE',  ( 48.97500000054622404, 22.36655054427230382, 83.50966788445364841 ) ) ;
#5628 = VECTOR ( 'NONE', #11218, 1000.000000000000000 ) ;
#5629 = CARTESIAN_POINT ( 'NONE',  ( 0.000000000000000000, 5.839897972853065333, -6.938893903907228378E-15 ) ) ;
#5630 = CARTESIAN_POINT ( 'NONE',  ( -3.767201726441450571, 53.30370413573731980, 24.71563014075751141 ) ) ;
#5631 = ORIENTED_EDGE ( 'NONE', *, *, #2384, .T. ) ;
#5632 = ORIENTED_EDGE ( 'NONE', *, *, #2201, .F. ) ;
#5633 = CARTESIAN_POINT ( 'NONE',  ( 27.49999999999999645, 20.00000000000000355, 172.0000000000000000 ) ) ;
#5634 = EDGE_CURVE ( 'NONE', #6052, #6404, #11143, .T. ) ;
#5635 =( BOUNDED_CURVE ( )  B_SPLINE_CURVE ( 2, ( #11944, #5096, #3307, #11052, #7883, #2360, #6109, #9979, #1288, #1100, #3249 ),
 .UNSPECIFIED., .F., .F. ) 
 B_SPLINE_CURVE_WITH_KNOTS ( ( 3, 2, 2, 2, 2, 3 ),
 ( 0.9666666666666666741, 0.9733333333333333837, 0.9799999999999999822, 0.9866666666666666918, 0.9933333333333332904, 1.000000000000000000 ),
 .UNSPECIFIED. ) 
 CURVE ( )  GEOMETRIC_REPRESENTATION_ITEM ( )  RATIONAL_B_SPLINE_CURVE ( ( 1.000000000000000000, 0.9510565162951535312, 1.000000000000000000, 0.9510565162951535312, 1.000000000000000000, 0.9510565162951535312, 1.000000000000000000, 0.9510565162951535312, 1.000000000000000000, 0.9510565162951535312, 1.000000000000000000 ) ) 
 REPRESENTATION_ITEM ( '' )  );
#5636 = DIRECTION ( 'NONE',  ( 0.000000000000000000, 0.8660254037844379305, -0.5000000000000012212 ) ) ;
#5637 = CARTESIAN_POINT ( 'NONE',  ( 34.87500000054622262, 20.00000000000000355, 83.50966788445364841 ) ) ;
#5638 = CARTESIAN_POINT ( 'NONE',  ( 19.87500000054622618, 17.63344945572769973, 98.07665518445361386 ) ) ;
#5639 = CARTESIAN_POINT ( 'NONE',  ( 12.59999999999999964, 8.082668874372530033E-16, 6.599999999999998757 ) ) ;
#5640 = PLANE ( 'NONE',  #10226 ) ;
#5641 = CARTESIAN_POINT ( 'NONE',  ( 2.510026038814216598, 45.66334912595792161, -20.85125448412398441 ) ) ;
#5642 = CARTESIAN_POINT ( 'NONE',  ( 3.304318396371782818, 46.23341735054634682, 27.80530896451984191 ) ) ;
#5643 = CIRCLE ( 'NONE', #4622, 25.00000000000000355 ) ;
#5644 = CARTESIAN_POINT ( 'NONE',  ( -2.000000000000015543, 20.00000000000000355, 90.79316153445363113 ) ) ;
#5645 = EDGE_LOOP ( 'NONE', ( #8468, #9144 ) ) ;
#5646 = CIRCLE ( 'NONE', #7263, 9.000000000000000000 ) ;
#5647 = CARTESIAN_POINT ( 'NONE',  ( 10.00000000000000355, 20.00000000000000355, -28.00000000000000711 ) ) ;
#5648 = CARTESIAN_POINT ( 'NONE',  ( 0.000000000000000000, 0.000000000000000000, 0.000000000000000000 ) ) ;
#5649 = AXIS2_PLACEMENT_3D ( 'NONE', #11817, #3823, #2043 ) ;
#5650 = CARTESIAN_POINT ( 'NONE',  ( 26.87500000054622618, 20.00000000000000355, 83.50966788445364841 ) ) ;
#5651 = FACE_OUTER_BOUND ( 'NONE', #3639, .T. ) ;
#5652 = CARTESIAN_POINT ( 'NONE',  ( 42.67500000054622689, 17.63344945572770328, 83.50966788445364841 ) ) ;
#5653 = CARTESIAN_POINT ( 'NONE',  ( 25.57500000054621836, 26.19570976099943493, 95.29460816699764791 ) ) ;
#5654 = CARTESIAN_POINT ( 'NONE',  ( 28.09999999999999076, 17.56310227825320425, 98.29316153445363113 ) ) ;
#5655 = ADVANCED_FACE ( 'NONE', ( #2516 ), #10012, .T. ) ;
#5656 = FILL_AREA_STYLE_COLOUR ( '', #11524 ) ;
#5657 = CARTESIAN_POINT ( 'NONE',  ( 41.17500000054623399, 26.92701409722686634, 88.54243821818162985 ) ) ;
#5658 = ORIENTED_EDGE ( 'NONE', *, *, #8626, .T. ) ;
#5659 = CARTESIAN_POINT ( 'NONE',  ( 46.67500000054623399, 17.63344945572770328, 83.50966788445364841 ) ) ;
#5660 = CARTESIAN_POINT ( 'NONE',  ( -4.838593727670618350, 48.69800932989790709, -20.43507704550293624 ) ) ;
#5661 = ORIENTED_EDGE ( 'NONE', *, *, #3044, .F. ) ;
#5662 = VECTOR ( 'NONE', #10650, 1000.000000000000000 ) ;
#5663 = PRODUCT_RELATED_PRODUCT_CATEGORY ( 'part', '', ( #8127 ) ) ;
#5664 = CARTESIAN_POINT ( 'NONE',  ( -6.102784694457409564, 27.94841462573825197, -27.33237746279936076 ) ) ;
#5665 = EDGE_CURVE ( 'NONE', #1603, #5036, #7084, .T. ) ;
#5666 = EDGE_LOOP ( 'NONE', ( #695, #4783, #743, #10363, #12092 ) ) ;
#5667 = AXIS2_PLACEMENT_3D ( 'NONE', #12204, #3504, #10289 ) ;
#5668 = CARTESIAN_POINT ( 'NONE',  ( 42.65000000109246514, 20.00000000000000355, 83.29316153445364534 ) ) ;
#5669 = CARTESIAN_POINT ( 'NONE',  ( 0.000000000000000000, 0.000000000000000000, 0.000000000000000000 ) ) ;
#5670 = CARTESIAN_POINT ( 'NONE',  ( 4.246185771498899975, 47.35493673757640920, -27.67631243003367558 ) ) ;
#5671 = CARTESIAN_POINT ( 'NONE',  ( 44.57500000054622546, 13.80429023900056684, 86.29171490190961435 ) ) ;
#5672 = DIRECTION ( 'NONE',  ( 1.000000000000000000, -0.000000000000000000, -0.000000000000000000 ) ) ;
#5673 = CARTESIAN_POINT ( 'NONE',  ( -1.299134361814098693, 45.16046244081530858, -27.97171976766272294 ) ) ;
#5674 = CARTESIAN_POINT ( 'NONE',  ( 45.97500000054623115, 17.63344945572769973, 98.07665518445361386 ) ) ;
#5675 = CARTESIAN_POINT ( 'NONE',  ( 47.09999999999999432, 22.43689772174679575, 83.29316153445363113 ) ) ;
#5676 = EDGE_CURVE ( 'NONE', #6680, #9812, #10075, .T. ) ;
#5677 = CARTESIAN_POINT ( 'NONE',  ( 41.09999999999998721, 22.43689772174679575, 83.29316153445363113 ) ) ;
#5678 = DIRECTION ( 'NONE',  ( 1.000000000000000000, 0.000000000000000000, 0.000000000000000000 ) ) ;
#5679 = ORIENTED_EDGE ( 'NONE', *, *, #4679, .T. ) ;
#5680 = CARTESIAN_POINT ( 'NONE',  ( 34.65000000109246514, 20.00000000000000355, 83.29316153445364534 ) ) ;
#5681 = CARTESIAN_POINT ( 'NONE',  ( 0.3310707342383826801, 55.00000000000000711, -24.99999999999999645 ) ) ;
#5682 = EDGE_LOOP ( 'NONE', ( #7404, #10172, #5991, #9860, #2960, #1874 ) ) ;
#5683 = EDGE_CURVE ( 'NONE', #12416, #1942, #6403, .T. ) ;
#5684 = VERTEX_POINT ( 'NONE', #7649 ) ;
#5685 = AXIS2_PLACEMENT_3D ( 'NONE', #4210, #1361, #8083 ) ;
#5686 = CARTESIAN_POINT ( 'NONE',  ( 121.0360000000000156, 7.347880794884120722E-16, -6.000000000000000888 ) ) ;
#5687 = FACE_OUTER_BOUND ( 'NONE', #607, .T. ) ;
#5688 = CARTESIAN_POINT ( 'NONE',  ( -9.983825383151277322, 20.65789756057008120, 22.91995855732452370 ) ) ;
#5689 = EDGE_CURVE ( 'NONE', #10115, #707, #928, .T. ) ;
#5690 = EDGE_CURVE ( 'NONE', #2755, #2795, #2762, .T. ) ;
#5691 = CARTESIAN_POINT ( 'NONE',  ( 90.00000000000000000, 0.000000000000000000, 0.000000000000000000 ) ) ;
#5692 = CARTESIAN_POINT ( 'NONE',  ( 21.99999999999998934, 20.00000000000000355, 98.29316153445363113 ) ) ;
#5693 = EDGE_LOOP ( 'NONE', ( #10189, #7109, #8456, #154 ) ) ;
#5694 = AXIS2_PLACEMENT_3D ( 'NONE', #5336, #2469, #392 ) ;
#5695 = DIRECTION ( 'NONE',  ( -1.000000000000000000, -0.000000000000000000, -0.000000000000000000 ) ) ;
#5696 = FACE_OUTER_BOUND ( 'NONE', #6366, .T. ) ;
#5697 = CARTESIAN_POINT ( 'NONE',  ( 49.07500000054622546, 24.28113015263587471, 84.90069139318163138 ) ) ;
#5698 = CARTESIAN_POINT ( 'NONE',  ( 50.99999999999997868, 20.00000000000000355, 170.0000000000000000 ) ) ;
#5699 = B_SPLINE_CURVE_WITH_KNOTS ( 'NONE', 3,
 ( #866, #10566, #9987, #8020, #9565, #1940, #6117, #1002, #2769, #7723, #5817, #11589, #4147, #12476, #1297, #2181, #6053, #4867 ),
 .UNSPECIFIED., .F., .F.,
 ( 4, 2, 2, 2, 2, 2, 2, 2, 4 ),
 ( 0.02353287092482041556, 0.02451293455144068142, 0.02549299817806094728, 0.02647306180468121314, 0.02745312543130147553, 0.02843318905792174139, 0.02941325268454200725, 0.03039331631116227311, 0.03137337993778253897 ),
 .UNSPECIFIED. ) ;
#5700 = FACE_OUTER_BOUND ( 'NONE', #10852, .T. ) ;
#5701 = VERTEX_POINT ( 'NONE', #7397 ) ;
#5702 = ORIENTED_EDGE ( 'NONE', *, *, #5360, .F. ) ;
#5703 = CARTESIAN_POINT ( 'NONE',  ( 21.39999999999998792, 27.13292387221364876, 88.47553407664153724 ) ) ;
#5704 = FACE_BOUND ( 'NONE', #11894, .T. ) ;
#5705 = CARTESIAN_POINT ( 'NONE',  ( 34.99999999999999289, 20.00000000000000355, 188.9999999999999716 ) ) ;
#5706 = DIRECTION ( 'NONE',  ( -0.000000000000000000, -1.000000000000000000, -0.000000000000000000 ) ) ;
#5707 = LINE ( 'NONE', #945, #3926 ) ;
#5708 = CARTESIAN_POINT ( 'NONE',  ( -21.00000000000001066, 77.00000000000000000, 154.3533255156881978 ) ) ;
#5709 = CARTESIAN_POINT ( 'NONE',  ( 25.85000000109246443, 15.59161060780645691, 96.86078899226572503 ) ) ;
#5710 = CARTESIAN_POINT ( 'NONE',  ( 3.061616998149962604E-15, 10.00000000000000000, 25.00000000000000000 ) ) ;
#5711 = ORIENTED_EDGE ( 'NONE', *, *, #10921, .F. ) ;
#5712 = DIRECTION ( 'NONE',  ( -1.000000000000000000, 0.000000000000000000, 0.000000000000000000 ) ) ;
#5713 = DIRECTION ( 'NONE',  ( -1.000000000000000000, 0.000000000000000000, 0.000000000000000000 ) ) ;
#5714 = CARTESIAN_POINT ( 'NONE',  ( 27.07500000054622546, 24.28113015263587471, 84.90069139318163138 ) ) ;
#5715 = CARTESIAN_POINT ( 'NONE',  ( 0.000000000000000000, 20.00000000000000355, 109.9999999999999858 ) ) ;
#5716 = CARTESIAN_POINT ( 'NONE',  ( 40.47500000054621694, 13.80429023900056684, 86.29171490190961435 ) ) ;
#5717 = CARTESIAN_POINT ( 'NONE',  ( 25.27500000054622475, 26.92701409722686634, 88.54243821818162985 ) ) ;
#5718 = CARTESIAN_POINT ( 'NONE',  ( 29.59999999999998721, 27.13292387221364876, 93.11078899226573924 ) ) ;
#5719 = PRESENTATION_STYLE_ASSIGNMENT (( #5843 ) ) ;
#5720 = CARTESIAN_POINT ( 'NONE',  ( 34.47500000054623115, 13.80429023900056684, 86.29171490190961435 ) ) ;
#5721 = EDGE_LOOP ( 'NONE', ( #407, #3695, #2412, #3670 ) ) ;
#5722 = CARTESIAN_POINT ( 'NONE',  ( 46.17500000054623399, 13.07298590277314254, 93.04388485072563242 ) ) ;
#5723 = CARTESIAN_POINT ( 'NONE',  ( -4.743665913102096177, 48.38584380519294825, -20.45762213685770092 ) ) ;
#5724 = EDGE_LOOP ( 'NONE', ( #5751, #5760, #12474, #7924, #469 ) ) ;
#5725 = EDGE_CURVE ( 'NONE', #2044, #2364, #6931, .T. ) ;
#5726 = B_SPLINE_CURVE_WITH_KNOTS ( 'NONE', 3,
 ( #6806, #11697, #8018, #5801, #7955, #1176, #7890, #9673, #3067, #281, #5102, #11821, #3129, #2941, #1109, #5926, #5865, #6996, #26, #10798 ),
 .UNSPECIFIED., .F., .F.,
 ( 4, 2, 2, 2, 2, 2, 2, 2, 2, 4 ),
 ( 0.01567185795944686308, 0.01665140573566027682, 0.01763095351187368709, 0.01812072739998039222, 0.01861050128808709736, 0.01959004906430051110, 0.02056959684051392484, 0.02154914461672733511, 0.02252869239294074538, 0.02350824016915415912 ),
 .UNSPECIFIED. ) ;
#5727 = CARTESIAN_POINT ( 'NONE',  ( 8.970506128821204683, 15.53268569158106871, 18.98970815876138118 ) ) ;
#5728 = VERTEX_POINT ( 'NONE', #8416 ) ;
#5729 = CARTESIAN_POINT ( 'NONE',  ( 6.000000000000000000, 2.919948986426540660, 5.057499999999996554 ) ) ;
#5730 = LINE ( 'NONE', #11313, #6034 ) ;
#5731 = CARTESIAN_POINT ( 'NONE',  ( 47.27500000054622831, 26.92701409722686634, 88.54243821818162985 ) ) ;
#5732 = CARTESIAN_POINT ( 'NONE',  ( 20.19999999999998863, 15.59161060780645691, 96.86078899226572503 ) ) ;
#5733 = CARTESIAN_POINT ( 'NONE',  ( 6.000000000000000000, -5.839897972853063557, 6.938893903907228378E-15 ) ) ;
#5734 = CARTESIAN_POINT ( 'NONE',  ( 44.77500000054622831, 17.63344945572770328, 83.50966788445364841 ) ) ;
#5735 = CARTESIAN_POINT ( 'NONE',  ( 48.99999999999998579, 20.00000000000000355, 83.29316153445364534 ) ) ;
#5736 = DIRECTION ( 'NONE',  ( 0.000000000000000000, -0.000000000000000000, -1.000000000000000000 ) ) ;
#5737 = CARTESIAN_POINT ( 'NONE',  ( -3.974987698915826595, 46.94954269600466290, 24.68264807992340337 ) ) ;
#5738 = VERTEX_POINT ( 'NONE', #8478 ) ;
#5739 = CIRCLE ( 'NONE', #673, 5.000000000000001776 ) ;
#5740 = CARTESIAN_POINT ( 'NONE',  ( 39.65000000109246514, 20.00000000000000355, 98.29316153445363113 ) ) ;
#5741 = DIRECTION ( 'NONE',  ( 0.000000000000000000, 0.000000000000000000, -1.000000000000000000 ) ) ;
#5742 = EDGE_LOOP ( 'NONE', ( #7247, #11998 ) ) ;
#5743 = CARTESIAN_POINT ( 'NONE',  ( -9.466558637120989772, 23.23925856829589520, -23.13860710034107626 ) ) ;
#5744 = ADVANCED_FACE ( 'NONE', ( #9497 ), #4729, .T. ) ;
#5745 = CARTESIAN_POINT ( 'NONE',  ( 6.000000000000000000, 0.000000000000000000, 0.000000000000000000 ) ) ;
#5746 = CARTESIAN_POINT ( 'NONE',  ( -6.109221465413982699, 27.94329460785578689, 24.24832107967536388 ) ) ;
#5747 = VECTOR ( 'NONE', #121, 1000.000000000000000 ) ;
#5748 = CARTESIAN_POINT ( 'NONE',  ( 36.47500000054622404, 13.80429023900056684, 86.29171490190961435 ) ) ;
#5749 = CARTESIAN_POINT ( 'NONE',  ( 34.72841614740048044, 22.00000000000000000, 169.9999999999999716 ) ) ;
#5750 = CARTESIAN_POINT ( 'NONE',  ( 27.19999999999998863, 24.40838939219355197, 84.72553407664153724 ) ) ;
#5751 = ORIENTED_EDGE ( 'NONE', *, *, #1502, .T. ) ;
#5752 = CARTESIAN_POINT ( 'NONE',  ( 5.000000000000002665, 50.32693827311778278, -27.54995462791183058 ) ) ;
#5753 = CARTESIAN_POINT ( 'NONE',  ( -5.299351711406078635, 11.51344256626987139, 27.49531132660919397 ) ) ;
#5754 = CARTESIAN_POINT ( 'NONE',  ( 23.17500000054622689, 26.92701409722686634, 88.54243821818162985 ) ) ;
#5755 = EDGE_LOOP ( 'NONE', ( #4580, #5711, #47, #2015 ) ) ;
#5756 = DIRECTION ( 'NONE',  ( 1.000000000000000000, -0.000000000000000000, -0.000000000000000000 ) ) ;
#5757 = AXIS2_PLACEMENT_3D ( 'NONE', #10803, #1116, #4020 ) ;
#5758 = CYLINDRICAL_SURFACE ( 'NONE', #4282, 7.499999999999992895 ) ;
#5759 = ORIENTED_EDGE ( 'NONE', *, *, #4726, .T. ) ;
#5760 = ORIENTED_EDGE ( 'NONE', *, *, #12423, .F. ) ;
#5761 = AXIS2_PLACEMENT_3D ( 'NONE', #2537, #2665, #6409 ) ;
#5762 = CARTESIAN_POINT ( 'NONE',  ( -1.331065827029258131, 29.93295003906536067, -20.96783762878424895 ) ) ;
#5763 = DIRECTION ( 'NONE',  ( 0.000000000000000000, 0.000000000000000000, -1.000000000000000000 ) ) ;
#5764 = EDGE_CURVE ( 'NONE', #5277, #9148, #6446, .T. ) ;
#5765 = CARTESIAN_POINT ( 'NONE',  ( 23.37500000054622973, 26.92701409722686634, 93.04388485072563242 ) ) ;
#5766 = CARTESIAN_POINT ( 'NONE',  ( -5.000000000000004441, 20.00000000000000000, 145.0000000000000000 ) ) ;
#5767 = CIRCLE ( 'NONE', #8205, 8.400000000000000355 ) ;
#5768 = CARTESIAN_POINT ( 'NONE',  ( -27.49999999999999645, 27.49999999999999645, 145.0000000000000000 ) ) ;
#5769 = CARTESIAN_POINT ( 'NONE',  ( 5.000000000000000000, 50.00000000000000000, -28.00000000000000711 ) ) ;
#5770 = CARTESIAN_POINT ( 'NONE',  ( 9.868178716563900110, 21.65205030131550146, -18.53711303768861640 ) ) ;
#5771 = CYLINDRICAL_SURFACE ( 'NONE', #11762, 7.499999999999992895 ) ;
#5772 = EDGE_LOOP ( 'NONE', ( #7767, #7420, #4230, #3336 ) ) ;
#5773 = CARTESIAN_POINT ( 'NONE',  ( 3.238656815135313671, 29.46670881375417395, -24.79134413122120151 ) ) ;
#5774 = SHAPE_DEFINITION_REPRESENTATION ( #226, #8235 ) ;
#5775 =( GEOMETRIC_REPRESENTATION_CONTEXT ( 3 ) GLOBAL_UNCERTAINTY_ASSIGNED_CONTEXT ( ( #7976 ) ) GLOBAL_UNIT_ASSIGNED_CONTEXT ( ( #11878, #8759, #76 ) ) REPRESENTATION_CONTEXT ( 'NONE', 'WORKASPACE' ) );
#5776 = CARTESIAN_POINT ( 'NONE',  ( 121.0360000000000156, 0.000000000000000000, 6.000000000000000888 ) ) ;
#5777 = CARTESIAN_POINT ( 'NONE',  ( 39.17500000054623399, 26.92701409722686634, 88.54243821818162985 ) ) ;
#5778 = CARTESIAN_POINT ( 'NONE',  ( 24.67500000054622689, 15.71886984736413773, 84.90069139318163138 ) ) ;
#5779 = CARTESIAN_POINT ( 'NONE',  ( 28.99999999999998934, 20.00000000000000355, 83.29316153445364534 ) ) ;
#5780 = DIRECTION ( 'NONE',  ( 1.000000000000000000, 0.000000000000000000, 0.000000000000000000 ) ) ;
#5781 = CARTESIAN_POINT ( 'NONE',  ( 35.47500000054623115, 26.19570976099943493, 95.29460816699764791 ) ) ;
#5782 = ORIENTED_EDGE ( 'NONE', *, *, #7927, .F. ) ;
#5783 = PRODUCT ( 'socket head cap screw_iso_ISO 4762 M10 x 80 - 32N', 'socket head cap screw_iso_ISO 4762 M10 x 80 - 32N', '', ( #3038 ) ) ;
#5784 = AXIS2_PLACEMENT_3D ( 'NONE', #432, #8171, #5379 ) ;
#5785 = DIRECTION ( 'NONE',  ( -1.000000000000000000, -0.000000000000000000, -0.000000000000000000 ) ) ;
#5786 = ORIENTED_EDGE ( 'NONE', *, *, #3179, .T. ) ;
#5787 = DIRECTION ( 'NONE',  ( -1.000000000000000000, -0.000000000000000000, -0.000000000000000000 ) ) ;
#5788 = ORIENTED_EDGE ( 'NONE', *, *, #3813, .F. ) ;
#5789 = CARTESIAN_POINT ( 'NONE',  ( 20.00000000000003908, 20.00000000000000000, 137.5000000000000000 ) ) ;
#5790 = VECTOR ( 'NONE', #7087, 1000.000000000000000 ) ;
#5791 = CARTESIAN_POINT ( 'NONE',  ( 8.666387210823231158, 14.96869202851870462, -26.62774317806001179 ) ) ;
#5792 = EDGE_CURVE ( 'NONE', #9392, #2848, #11391, .T. ) ;
#5793 = CARTESIAN_POINT ( 'NONE',  ( 44.47500000054622404, 13.07298590277314432, 88.54243821818161564 ) ) ;
#5794 = CYLINDRICAL_SURFACE ( 'NONE', #496, 7.499999999999992895 ) ;
#5795 = EDGE_CURVE ( 'NONE', #5802, #1127, #9742, .T. ) ;
#5796 = CARTESIAN_POINT ( 'NONE',  ( 45.27500000054622831, 26.92701409722686634, 88.54243821818162985 ) ) ;
#5797 = CARTESIAN_POINT ( 'NONE',  ( 20.77500000054622120, 17.63344945572770328, 83.50966788445364841 ) ) ;
#5798 = CARTESIAN_POINT ( 'NONE',  ( 44.39999999999999147, 12.86707612778636012, 93.11078899226572503 ) ) ;
#5799 = ORIENTED_EDGE ( 'NONE', *, *, #8944, .T. ) ;
#5800 = CARTESIAN_POINT ( 'NONE',  ( 30.15000000109246159, 12.11403331821300533, 90.79316153445363113 ) ) ;
#5801 = CARTESIAN_POINT ( 'NONE',  ( 1.300123024442352504, 45.16070347875686508, -24.96827571664099565 ) ) ;
#5802 = VERTEX_POINT ( 'NONE', #7461 ) ;
#5803 = ORIENTED_EDGE ( 'NONE', *, *, #5689, .F. ) ;
#5804 = CYLINDRICAL_SURFACE ( 'NONE', #4850, 7.499999999999992895 ) ;
#5805 = LINE ( 'NONE', #9930, #4206 ) ;
#5806 = DIRECTION ( 'NONE',  ( 1.000000000000000000, -0.000000000000000000, -0.000000000000000000 ) ) ;
#5807 = AXIS2_PLACEMENT_3D ( 'NONE', #4246, #4426, #12113 ) ;
#5808 = CARTESIAN_POINT ( 'NONE',  ( 35.37500000054622973, 26.92701409722686634, 93.04388485072563242 ) ) ;
#5809 = CARTESIAN_POINT ( 'NONE',  ( 3.429011071898990822E-15, 55.00000000000000000, 28.00000000000000355 ) ) ;
#5810 = CARTESIAN_POINT ( 'NONE',  ( 27.50000000000000355, 27.49999999999999645, 145.0000000000000000 ) ) ;
#5811 = ORIENTED_EDGE ( 'NONE', *, *, #261, .T. ) ;
#5812 = EDGE_CURVE ( 'NONE', #4895, #3111, #2701, .T. ) ;
#5813 = CARTESIAN_POINT ( 'NONE',  ( 4.339334521168333403, 52.50564928449409052, -27.66232676752730768 ) ) ;
#5814 = CARTESIAN_POINT ( 'NONE',  ( 0.3310707342383826801, 55.00000000000000711, -24.99999999999999645 ) ) ;
#5815 = CARTESIAN_POINT ( 'NONE',  ( 48.07500000054622546, 15.71886984736413417, 96.68563167572563088 ) ) ;
#5816 = VERTEX_POINT ( 'NONE', #7526 ) ;
#5817 = CARTESIAN_POINT ( 'NONE',  ( 3.054638161218191872, 53.97201501934328149, -20.77847170131455456 ) ) ;
#5818 = VERTEX_POINT ( 'NONE', #6567 ) ;
#5819 = VECTOR ( 'NONE', #3754, 1000.000000000000000 ) ;
#5820 = PRODUCT_RELATED_PRODUCT_CATEGORY ( 'part', '', ( #5086 ) ) ;
#5821 = CARTESIAN_POINT ( 'NONE',  ( 27.49999999999999645, 20.00000000000000355, 170.9999999999999716 ) ) ;
#5822 = EDGE_CURVE ( 'NONE', #1088, #6810, #2214, .T. ) ;
#5823 = CARTESIAN_POINT ( 'NONE',  ( -5.855196281420844251, 28.11311675345165995, -20.16916341828400761 ) ) ;
#5824 = CARTESIAN_POINT ( 'NONE',  ( -10.00000000000000355, 20.00000000000000355, 26.15339366124404208 ) ) ;
#5825 = CIRCLE ( 'NONE', #7654, 4.057500000000000107 ) ;
#5826 = CARTESIAN_POINT ( 'NONE',  ( 23.47500000054622760, 26.19570976099943849, 95.29460816699764791 ) ) ;
#5827 = CARTESIAN_POINT ( 'NONE',  ( 29.99999999999998934, 20.00000000000000355, 98.29316153445363113 ) ) ;
#5828 = FACE_OUTER_BOUND ( 'NONE', #984, .T. ) ;
#5829 = LINE ( 'NONE', #11535, #10199 ) ;
#5830 = CARTESIAN_POINT ( 'NONE',  ( 9.983699295846122368, 20.66008309228626771, -18.47504095581592409 ) ) ;
#5831 = CARTESIAN_POINT ( 'NONE',  ( 6.000000000000000000, -2.919948986426523341, 5.057500000000002771 ) ) ;
#5832 = EDGE_LOOP ( 'NONE', ( #12243, #2195, #1253 ) ) ;
#5833 = LINE ( 'NONE', #6711, #10693 ) ;
#5834 = EDGE_CURVE ( 'NONE', #10526, #9490, #4668, .T. ) ;
#5835 = SHAPE_DEFINITION_REPRESENTATION ( #10056, #10013 ) ;
#5836 = CARTESIAN_POINT ( 'NONE',  ( 27.67500000054622333, 24.28113015263587116, 96.68563167572563088 ) ) ;
#5837 = CARTESIAN_POINT ( 'NONE',  ( 6.000000000000000000, 0.000000000000000000, 0.000000000000000000 ) ) ;
#5838 = CARTESIAN_POINT ( 'NONE',  ( 41.37500000054622262, 26.92701409722686634, 93.04388485072563242 ) ) ;
#5839 = ADVANCED_FACE ( 'NONE', ( #7713 ), #2003, .F. ) ;
#5840 = VECTOR ( 'NONE', #7030, 1000.000000000000114 ) ;
#5841 = CARTESIAN_POINT ( 'NONE',  ( 28.87500000054622262, 20.00000000000000355, 83.50966788445364841 ) ) ;
#5842 = CARTESIAN_POINT ( 'NONE',  ( 23.99999999999998579, 20.00000000000000355, 98.29316153445363113 ) ) ;
#5843 = SURFACE_STYLE_USAGE ( .BOTH. , #5595 ) ;
#5844 = CARTESIAN_POINT ( 'NONE',  ( 33.27500000054621410, 27.65831843345427998, 90.79316153445363113 ) ) ;
#5845 = ORIENTED_EDGE ( 'NONE', *, *, #11027, .T. ) ;
#5846 = FACE_OUTER_BOUND ( 'NONE', #1437, .T. ) ;
#5847 = VERTEX_POINT ( 'NONE', #12531 ) ;
#5848 = CARTESIAN_POINT ( 'NONE',  ( 0.000000000000000000, 0.000000000000000000, 0.000000000000000000 ) ) ;
#5849 = ORIENTED_EDGE ( 'NONE', *, *, #8928, .T. ) ;
#5850 =( BOUNDED_CURVE ( )  B_SPLINE_CURVE ( 2, ( #10360, #1796, #12279, #12338, #7702, #3698, #7641, #9426, #4657, #3636, #4785 ),
 .UNSPECIFIED., .F., .F. ) 
 B_SPLINE_CURVE_WITH_KNOTS ( ( 3, 2, 2, 2, 2, 3 ),
 ( 0.8333333333333333703, 0.8399999999999999689, 0.8466666666666666785, 0.8533333333333333881, 0.8599999999999999867, 0.8666666666666666963 ),
 .UNSPECIFIED. ) 
 CURVE ( )  GEOMETRIC_REPRESENTATION_ITEM ( )  RATIONAL_B_SPLINE_CURVE ( ( 1.000000000000000000, 0.9510565162951535312, 1.000000000000000000, 0.9510565162951535312, 1.000000000000000000, 0.9510565162951535312, 1.000000000000000000, 0.9510565162951535312, 1.000000000000000000, 0.9510565162951535312, 1.000000000000000000 ) ) 
 REPRESENTATION_ITEM ( '' )  );
#5851 =( NAMED_UNIT ( * ) PLANE_ANGLE_UNIT ( ) SI_UNIT ( $, .RADIAN. ) );
#5852 = VECTOR ( 'NONE', #11756, 1000.000000000000000 ) ;
#5853 = CARTESIAN_POINT ( 'NONE',  ( 43.19999999999998863, 24.40838939219355197, 84.72553407664153724 ) ) ;
#5854 = CARTESIAN_POINT ( 'NONE',  ( 0.000000000000000000, 139.9999999999999716, -21.00000000000000000 ) ) ;
#5855=STYLED_ITEM('',(#12591),#1830);
#5856 = CARTESIAN_POINT ( 'NONE',  ( 46.77500000054622831, 17.63344945572770328, 83.50966788445364841 ) ) ;
#5857 = DIRECTION ( 'NONE',  ( -0.000000000000000000, -0.000000000000000000, 1.000000000000000000 ) ) ;
#5858 = CARTESIAN_POINT ( 'NONE',  ( 0.000000000000000000, 0.000000000000000000, 169.9999999999999716 ) ) ;
#5859 = CARTESIAN_POINT ( 'NONE',  ( 46.27500000054622831, 13.07298590277314254, 93.04388485072563242 ) ) ;
#5860 = CARTESIAN_POINT ( 'NONE',  ( 44.69999999999998153, 13.62011893735971135, 86.15790661882942914 ) ) ;
#5861 = CARTESIAN_POINT ( 'NONE',  ( 38.99999999999998579, 20.00000000000000355, 83.29316153445364534 ) ) ;
#5862 = CARTESIAN_POINT ( 'NONE',  ( -6.999999999999999112, 84.49999999999998579, 146.8533255156881978 ) ) ;
#5863 = ORIENTED_EDGE ( 'NONE', *, *, #2414, .T. ) ;
#5864 = CARTESIAN_POINT ( 'NONE',  ( 31.45000000109246585, 24.40838939219354842, 96.86078899226572503 ) ) ;
#5865 = CARTESIAN_POINT ( 'NONE',  ( 4.839602763736350788, 48.70207075804894714, -24.52717836283222752 ) ) ;
#5866 = ORIENTED_EDGE ( 'NONE', *, *, #4562, .F. ) ;
#5867 = CIRCLE ( 'NONE', #5261, 26.49999999999999645 ) ;
#5868 = ORIENTED_EDGE ( 'NONE', *, *, #4791, .T. ) ;
#5869 = CARTESIAN_POINT ( 'NONE',  ( -5.033342733373901368, 28.66546597776486038, -24.49435860509168350 ) ) ;
#5870 = DIRECTION ( 'NONE',  ( 0.000000000000000000, -1.039664082171044875E-15, -1.000000000000000000 ) ) ;
#5871 = CARTESIAN_POINT ( 'NONE',  ( 37.97500000054623115, 15.71886984736413417, 96.68563167572563088 ) ) ;
#5872 = CARTESIAN_POINT ( 'NONE',  ( 41.07500000054622546, 24.28113015263587471, 84.90069139318163138 ) ) ;
#5873 = DIRECTION ( 'NONE',  ( -0.000000000000000000, -0.000000000000000000, 1.000000000000000000 ) ) ;
#5874 = CARTESIAN_POINT ( 'NONE',  ( -9.867139490978726002, 21.65793074649777594, 18.53766545382552167 ) ) ;
#5875 = DIRECTION ( 'NONE',  ( 1.000000000000000000, -0.000000000000000000, -0.000000000000000000 ) ) ;
#5876 = ORIENTED_EDGE ( 'NONE', *, *, #791, .T. ) ;
#5877 = CARTESIAN_POINT ( 'NONE',  ( 3.651743720672741667, 53.41923203171982237, -24.73212923346887848 ) ) ;
#5878 = CARTESIAN_POINT ( 'NONE',  ( 46.99999999999998579, 20.00000000000000355, 83.29316153445364534 ) ) ;
#5879 = ORIENTED_EDGE ( 'NONE', *, *, #8703, .F. ) ;
#5880 = CARTESIAN_POINT ( 'NONE',  ( 0.000000000000000000, -4.262400816306111331E-15, 0.000000000000000000 ) ) ;
#5881 = AXIS2_PLACEMENT_3D ( 'NONE', #3444, #6175, #10228 ) ;
#5882 = VERTEX_POINT ( 'NONE', #6064 ) ;
#5883 = ADVANCED_FACE ( 'NONE', ( #7900 ), #5936, .T. ) ;
#5884 = EDGE_LOOP ( 'NONE', ( #5600, #5845, #12186, #2522 ) ) ;
#5885 = DIRECTION ( 'NONE',  ( -0.7071067811865342501, 8.659560562355096793E-17, -0.7071067811865608954 ) ) ;
#5886 = EDGE_CURVE ( 'NONE', #113, #5882, #9337, .T. ) ;
#5887 = AXIS2_PLACEMENT_3D ( 'NONE', #5831, #9830, #2076 ) ;
#5888 = DIRECTION ( 'NONE',  ( 0.000000000000000000, 1.000000000000000000, 0.000000000000000000 ) ) ;
#5889 = DIRECTION ( 'NONE',  ( -1.000000000000000000, -0.000000000000000000, -0.000000000000000000 ) ) ;
#5890 = CYLINDRICAL_SURFACE ( 'NONE', #1205, 7.499999999999992895 ) ;
#5891 = CARTESIAN_POINT ( 'NONE',  ( 10.00000000000000355, 20.67071788932440413, 18.46618531261938756 ) ) ;
#5892 = CARTESIAN_POINT ( 'NONE',  ( -4.743108530676050982, 51.61529827254528158, 20.45774488160513371 ) ) ;
#5893 = EDGE_CURVE ( 'NONE', #10229, #6052, #10870, .T. ) ;
#5894 = DIRECTION ( 'NONE',  ( -1.000000000000000000, -0.000000000000000000, -0.000000000000000000 ) ) ;
#5895 = DIRECTION ( 'NONE',  ( 1.000000000000000000, -0.000000000000000000, -0.000000000000000000 ) ) ;
#5896 = ORIENTED_EDGE ( 'NONE', *, *, #9071, .T. ) ;
#5897 = AXIS2_PLACEMENT_3D ( 'NONE', #8209, #3258, #11061 ) ;
#5898 = CARTESIAN_POINT ( 'NONE',  ( 9.355409448593292154, 23.54720254436722371, -23.18392859692124830 ) ) ;
#5899 = APPLICATION_PROTOCOL_DEFINITION ( 'draft international standard', 'automotive_design', 1998, #7801 ) ;
#5900 = EDGE_CURVE ( 'NONE', #12462, #5355, #8786, .T. ) ;
#5901 = CARTESIAN_POINT ( 'NONE',  ( 46.79999999999999005, 15.59161060780646046, 84.72553407664153724 ) ) ;
#5902 = CARTESIAN_POINT ( 'NONE',  ( 48.67500000054622689, 15.71886984736413773, 84.90069139318163138 ) ) ;
#5903 = CARTESIAN_POINT ( 'NONE',  ( 33.67500000054622689, 22.36655054427230027, 98.07665518445361386 ) ) ;
#5904 = CARTESIAN_POINT ( 'NONE',  ( 20.77500000054622120, 17.63344945572770328, 83.50966788445364841 ) ) ;
#5905 = CARTESIAN_POINT ( 'NONE',  ( 22.99999999999998934, 20.00000000000000355, 83.29316153445364534 ) ) ;
#5906 = AXIS2_PLACEMENT_3D ( 'NONE', #4754, #7612, #10452 ) ;
#5907 = EDGE_CURVE ( 'NONE', #2444, #4011, #3732, .T. ) ;
#5908 = CARTESIAN_POINT ( 'NONE',  ( 48.99999999999998579, 20.00000000000000355, 83.29316153445364534 ) ) ;
#5909 = CARTESIAN_POINT ( 'NONE',  ( 30.17500000054623044, 13.07298590277314254, 93.04388485072563242 ) ) ;
#5910 = VERTEX_POINT ( 'NONE', #11301 ) ;
#5911 = DIRECTION ( 'NONE',  ( 0.000000000000000000, -0.5000000000000014433, -0.8660254037844379305 ) ) ;
#5912 = ORIENTED_EDGE ( 'NONE', *, *, #2205, .F. ) ;
#5913 = VERTEX_POINT ( 'NONE', #4510 ) ;
#5914 = EDGE_CURVE ( 'NONE', #10184, #3396, #3655, .T. ) ;
#5915 = LINE ( 'NONE', #9784, #10639 ) ;
#5916 = CARTESIAN_POINT ( 'NONE',  ( 8.124733646131113929, 14.16101164777853150, -26.79597818126044473 ) ) ;
#5917 = CARTESIAN_POINT ( 'NONE',  ( 37.07500000054622546, 24.28113015263587471, 84.90069139318163138 ) ) ;
#5918 = CYLINDRICAL_SURFACE ( 'NONE', #6740, 7.499999999999992895 ) ;
#5919 = CARTESIAN_POINT ( 'NONE',  ( -3.294598684565033704E-22, 45.00000000000000711, -28.00000000000000355 ) ) ;
#5920 = CARTESIAN_POINT ( 'NONE',  ( 37.37500000054622262, 27.65831843345427998, 90.79316153445363113 ) ) ;
#5921 = CARTESIAN_POINT ( 'NONE',  ( 44.79999999999998295, 15.59161060780646046, 84.72553407664153724 ) ) ;
#5922 = CARTESIAN_POINT ( 'NONE',  ( -9.935193375007562722, 21.31442233758455274, -22.94148538850174646 ) ) ;
#5923 = CARTESIAN_POINT ( 'NONE',  ( 0.000000000000000000, 20.00000000000000355, -28.00000000000000711 ) ) ;
#5924 = ORIENTED_EDGE ( 'NONE', *, *, #10368, .F. ) ;
#5925 = CARTESIAN_POINT ( 'NONE',  ( 28.45000000109246585, 15.59161060780646046, 84.72553407664153724 ) ) ;
#5926 = CARTESIAN_POINT ( 'NONE',  ( 4.743618752923510762, 48.38567045510036735, -24.54617134760821173 ) ) ;
#5927 = ORIENTED_EDGE ( 'NONE', *, *, #9679, .F. ) ;
#5928 =( BOUNDED_CURVE ( )  B_SPLINE_CURVE ( 2, ( #12389, #6667, #969, #4838, #9722, #7751, #8705, #13, #5853, #9476, #7815 ),
 .UNSPECIFIED., .F., .F. ) 
 B_SPLINE_CURVE_WITH_KNOTS ( ( 3, 2, 2, 2, 2, 3 ),
 ( 0.1999999999999999278, 0.2066666666666665819, 0.2133333333333332915, 0.2199999999999999456, 0.2266666666666666274, 0.2333333333333333093 ),
 .UNSPECIFIED. ) 
 CURVE ( )  GEOMETRIC_REPRESENTATION_ITEM ( )  RATIONAL_B_SPLINE_CURVE ( ( 1.000000000000000666, 0.9510565162951528650, 1.000000000000000000, 0.9510565162951535312, 1.000000000000000000, 0.9510565162951535312, 1.000000000000000000, 0.9510565162951535312, 1.000000000000000000, 0.9510565162951537532, 0.9999999999999997780 ) ) 
 REPRESENTATION_ITEM ( '' )  );
#5929 = VERTEX_POINT ( 'NONE', #2606 ) ;
#5930 = CARTESIAN_POINT ( 'NONE',  ( -10.00000000000000533, 20.66054119461773553, -22.91287847477919470 ) ) ;
#5931 = CARTESIAN_POINT ( 'NONE',  ( 6.000000000000000000, 2.919948986426526005, -5.057500000000003659 ) ) ;
#5932 = DIRECTION ( 'NONE',  ( 0.000000000000000000, 0.000000000000000000, 1.000000000000000000 ) ) ;
#5933 = CARTESIAN_POINT ( 'NONE',  ( 35.87500000054622262, 17.63344945572769973, 98.07665518445361386 ) ) ;
#5934 = CARTESIAN_POINT ( 'NONE',  ( 34.07500000054622546, 15.71886984736413417, 96.68563167572563088 ) ) ;
#5935 = CIRCLE ( 'NONE', #4921, 7.499999999999978684 ) ;
#5936 = PLANE ( 'NONE',  #8491 ) ;
#5937 = DIRECTION ( 'NONE',  ( 0.000000000000000000, 0.000000000000000000, 1.000000000000000000 ) ) ;
#5938 = ORIENTED_EDGE ( 'NONE', *, *, #10663, .F. ) ;
#5939 = CARTESIAN_POINT ( 'NONE',  ( 47.65000000109246514, 20.00000000000000355, 98.29316153445363113 ) ) ;
#5940 = ORIENTED_EDGE ( 'NONE', *, *, #7973, .T. ) ;
#5941 = CARTESIAN_POINT ( 'NONE',  ( 0.000000000000000000, 20.00000000000000355, -28.00000000000000711 ) ) ;
#5942 = EDGE_LOOP ( 'NONE', ( #11633, #8084, #4288, #4988 ) ) ;
#5943 = ORIENTED_EDGE ( 'NONE', *, *, #7862, .F. ) ;
#5944 = VECTOR ( 'NONE', #9309, 1000.000000000000000 ) ;
#5945 = LINE ( 'NONE', #10821, #3171 ) ;
#5946 = DIRECTION ( 'NONE',  ( 0.000000000000000000, 0.000000000000000000, -1.000000000000000000 ) ) ;
#5947 = CARTESIAN_POINT ( 'NONE',  ( 20.27158385259953377, 22.00000000000000000, 152.2284161474004520 ) ) ;
#5948 = EDGE_CURVE ( 'NONE', #12211, #11194, #2689, .T. ) ;
#5949 = CARTESIAN_POINT ( 'NONE',  ( 10.00000000000000000, 0.000000000000000000, 0.000000000000000000 ) ) ;
#5950 = AXIS2_PLACEMENT_3D ( 'NONE', #907, #4777, #12269 ) ;
#5951 = CARTESIAN_POINT ( 'NONE',  ( 1.342157722727130131E-15, 30.00000000000002132, -21.00000000000000355 ) ) ;
#5952 = CARTESIAN_POINT ( 'NONE',  ( 4.743517746076369335, 48.38525476062307717, -20.45765889729212716 ) ) ;
#5953 = DIRECTION ( 'NONE',  ( -1.000000000000000000, -0.000000000000000000, -0.000000000000000000 ) ) ;
#5954 = CARTESIAN_POINT ( 'NONE',  ( 41.07500000054622546, 26.19570976099943493, 86.29171490190961435 ) ) ;
#5955 = AXIS2_PLACEMENT_3D ( 'NONE', #12188, #3488, #11294 ) ;
#5956 = LINE ( 'NONE', #6841, #12171 ) ;
#5957 = ORIENTED_EDGE ( 'NONE', *, *, #4429, .T. ) ;
#5958 = CARTESIAN_POINT ( 'NONE',  ( -2.615680359617244211, 10.32552686981736123, -27.88513211093687971 ) ) ;
#5959 = SHAPE_DEFINITION_REPRESENTATION ( #4059, #7408 ) ;
#5960 = LINE ( 'NONE', #9836, #11890 ) ;
#5961 = CARTESIAN_POINT ( 'NONE',  ( 6.000000000000000000, 0.000000000000000000, 0.000000000000000000 ) ) ;
#5962 = CARTESIAN_POINT ( 'NONE',  ( 32.67500000054622689, 17.63344945572770328, 83.50966788445364841 ) ) ;
#5963 = DIRECTION ( 'NONE',  ( 0.000000000000000000, 1.000000000000000000, 0.000000000000000000 ) ) ;
#5964 = CARTESIAN_POINT ( 'NONE',  ( 23.39999999999998792, 27.13292387221364876, 88.47553407664153724 ) ) ;
#5965 = CYLINDRICAL_SURFACE ( 'NONE', #3021, 7.499999999999992895 ) ;
#5966 = CARTESIAN_POINT ( 'NONE',  ( 34.57500000054623257, 15.71886984736413773, 84.90069139318163138 ) ) ;
#5967 = ORIENTED_EDGE ( 'NONE', *, *, #1568, .T. ) ;
#5968 = EDGE_CURVE ( 'NONE', #4064, #7564, #12194, .T. ) ;
#5969 = PLANE ( 'NONE',  #9334 ) ;
#5970 = CARTESIAN_POINT ( 'NONE',  ( -10.00000000000000355, 20.00000000000000355, -18.46618531261938401 ) ) ;
#5971 = ORIENTED_EDGE ( 'NONE', *, *, #3642, .F. ) ;
#5972 = CARTESIAN_POINT ( 'NONE',  ( 49.35000000109246798, 26.37988106264029398, 95.42841645007781892 ) ) ;
#5973 = ORIENTED_EDGE ( 'NONE', *, *, #5297, .F. ) ;
#5974 = LINE ( 'NONE', #5091, #6794 ) ;
#5975 = DIRECTION ( 'NONE',  ( 1.000000000000000000, -0.000000000000000000, -0.000000000000000000 ) ) ;
#5976 = CARTESIAN_POINT ( 'NONE',  ( 35.77500000054622831, 22.36655054427230027, 98.07665518445361386 ) ) ;
#5977 = CARTESIAN_POINT ( 'NONE',  ( 7.342598717236928252, 0.000000000000000000, 0.000000000000000000 ) ) ;
#5979 = CARTESIAN_POINT ( 'NONE',  ( 49.57500000054623257, 24.28113015263587116, 96.68563167572563088 ) ) ;
#5978 = B_SPLINE_CURVE_WITH_KNOTS ( 'NONE', 3,
 ( #1071, #11980, #4935, #9826, #8803, #8048, #4104, #5069, #8934, #11916, #120, #7085, #1324, #2274, #7983, #3159, #8867, #5195, #4041, #10016 ),
 .UNSPECIFIED., .F., .F.,
 ( 4, 2, 2, 2, 2, 2, 2, 2, 2, 4 ),
 ( 0.007837888240810860288, 0.008817134455640363022, 0.009796380670469867491, 0.01028600377788460932, 0.01077562688529935114, 0.01175487310012885388, 0.01273411931495835661, 0.01371336552978785761, 0.01469261174461736208, 0.01567185795944686308 ),
 .UNSPECIFIED. ) ;
#5980 = CARTESIAN_POINT ( 'NONE',  ( 41.97500000054623115, 17.63344945572769973, 98.07665518445361386 ) ) ;
#5981 = CARTESIAN_POINT ( 'NONE',  ( 45.49999999999997868, 27.88596668178699645, 90.79316153445363113 ) ) ;
#5982 = VECTOR ( 'NONE', #4416, 1000.000000000000000 ) ;
#5983 = DIRECTION ( 'NONE',  ( -0.000000000000000000, -0.000000000000000000, 1.000000000000000000 ) ) ;
#5984 = DIRECTION ( 'NONE',  ( -1.000000000000000000, 0.000000000000000000, 0.000000000000000000 ) ) ;
#5985 = ORIENTED_EDGE ( 'NONE', *, *, #10711, .F. ) ;
#5986 = EDGE_CURVE ( 'NONE', #8006, #6176, #1596, .T. ) ;
#5987 = CARTESIAN_POINT ( 'NONE',  ( 29.25000000109246301, 27.13292387221364876, 93.11078899226573924 ) ) ;
#5988 = DIRECTION ( 'NONE',  ( 0.000000000000000000, -0.5000000000000011102, -0.8660254037844379305 ) ) ;
#5989 = VERTEX_POINT ( 'NONE', #2260 ) ;
#5990 = AXIS2_PLACEMENT_3D ( 'NONE', #11787, #2276, #9891 ) ;
#5991 = ORIENTED_EDGE ( 'NONE', *, *, #10351, .T. ) ;
#5992 = CARTESIAN_POINT ( 'NONE',  ( 9.741406019701777552, 17.71702429258190747, 26.25089909648496089 ) ) ;
#5993 = PRODUCT ( 'Bolt-Mounted Retaining Cylinder', 'Bolt-Mounted Retaining Cylinder', '', ( #1210 ) ) ;
#5994 = EDGE_CURVE ( 'NONE', #1407, #7179, #9107, .T. ) ;
#5995 = DIRECTION ( 'NONE',  ( 0.000000000000000000, 0.000000000000000000, 1.000000000000000000 ) ) ;
#5996 = LINE ( 'NONE', #10678, #7170 ) ;
#5997 = CARTESIAN_POINT ( 'NONE',  ( 28.37500000054622618, 13.07298590277314432, 88.54243821818161564 ) ) ;
#5998 = CARTESIAN_POINT ( 'NONE',  ( 32.37500000054621552, 12.34168156654572535, 90.79316153445363113 ) ) ;
#5999 = CARTESIAN_POINT ( 'NONE',  ( 46.65000000109246514, 20.00000000000000355, 83.29316153445364534 ) ) ;
#6000 = EDGE_CURVE ( 'NONE', #4846, #12355, #8263, .T. ) ;
#6001 = CARTESIAN_POINT ( 'NONE',  ( 3.548616897151023686, 29.35492511944846683, -27.77589733847015552 ) ) ;
#6002 = VERTEX_POINT ( 'NONE', #765 ) ;
#6003 = CIRCLE ( 'NONE', #9653, 9.000000000000000000 ) ;
#6004 = CARTESIAN_POINT ( 'NONE',  ( 4.493076325134499172, 52.21789521489533570, -24.59326131088672440 ) ) ;
#6005 = CARTESIAN_POINT ( 'NONE',  ( -50.00000000000001421, 0.000000000000000000, 169.9999999999999716 ) ) ;
#6006 = EDGE_LOOP ( 'NONE', ( #2410, #3239 ) ) ;
#6007 = FACE_OUTER_BOUND ( 'NONE', #9286, .T. ) ;
#6008 = ORIENTED_EDGE ( 'NONE', *, *, #8425, .T. ) ;
#6009 = LINE ( 'NONE', #6424, #1708 ) ;
#6010 = CARTESIAN_POINT ( 'NONE',  ( -10.00000000000000178, 19.66809010557521020, -18.46618531261939111 ) ) ;
#6011 = DIRECTION ( 'NONE',  ( 0.000000000000000000, 0.000000000000000000, -1.000000000000000000 ) ) ;
#6012 = LINE ( 'NONE', #10757, #10078 ) ;
#6013 = CARTESIAN_POINT ( 'NONE',  ( 9.949532711038518329, 21.03606021117587233, 83.36056314470675943 ) ) ;
#6014 = LINE ( 'NONE', #9888, #3419 ) ;
#6015 = CARTESIAN_POINT ( 'NONE',  ( 3.257619892980143650, 29.47720406012850347, 20.75490610440258621 ) ) ;
#6016 = CARTESIAN_POINT ( 'NONE',  ( 0.000000000000000000, 2.919948986426539772, 5.057499999999996554 ) ) ;
#6017 = VECTOR ( 'NONE', #8106, 1000.000000000000000 ) ;
#6018 = CARTESIAN_POINT ( 'NONE',  ( -4.743629175984715118, 48.38625991566029683, 27.59554290692945600 ) ) ;
#6019 = CARTESIAN_POINT ( 'NONE',  ( 42.97500000054623115, 24.28113015263587471, 84.90069139318163138 ) ) ;
#6020 = CARTESIAN_POINT ( 'NONE',  ( 0.3275525315169112162, 44.99999999999999289, 20.99999999999999645 ) ) ;
#6021 = ORIENTED_EDGE ( 'NONE', *, *, #729, .T. ) ;
#6022 = CARTESIAN_POINT ( 'NONE',  ( 37.15000000109246514, 27.88596668178699645, 90.79316153445363113 ) ) ;
#6023 = EDGE_CURVE ( 'NONE', #527, #10184, #8695, .T. ) ;
#6024 = AXIS2_PLACEMENT_3D ( 'NONE', #4809, #8677, #8783 ) ;
#6025 = CARTESIAN_POINT ( 'NONE',  ( 23.27500000054622475, 26.92701409722686634, 88.54243821818162985 ) ) ;
#6026 = CARTESIAN_POINT ( 'NONE',  ( 0.6000000000000033085, 1.028703311283776586E-15, -8.400000000000000355 ) ) ;
#6027 = CARTESIAN_POINT ( 'NONE',  ( 32.87500000054622973, 22.36655054427230382, 83.50966788445364841 ) ) ;
#6028 = CARTESIAN_POINT ( 'NONE',  ( 6.114177788104627531, 12.06044222946883693, -24.24708634001311580 ) ) ;
#6029 = CARTESIAN_POINT ( 'NONE',  ( 24.69999999999998508, 13.62011893735971135, 86.15790661882942914 ) ) ;
#6030 = DIRECTION ( 'NONE',  ( 1.000000000000000000, -0.000000000000000000, -0.000000000000000000 ) ) ;
#6031 = CARTESIAN_POINT ( 'NONE',  ( 24.37500000054622618, 13.07298590277314432, 88.54243821818161564 ) ) ;
#6032 = ORIENTED_EDGE ( 'NONE', *, *, #11173, .F. ) ;
#6033 = ORIENTED_EDGE ( 'NONE', *, *, #4314, .F. ) ;
#6034 = VECTOR ( 'NONE', #2620, 1000.000000000000000 ) ;
#6035 = ORIENTED_EDGE ( 'NONE', *, *, #10610, .F. ) ;
#6036 = DIRECTION ( 'NONE',  ( -0.000000000000000000, -0.000000000000000000, 1.000000000000000000 ) ) ;
#6037 = ORIENTED_EDGE ( 'NONE', *, *, #2113, .T. ) ;
#6038 = CARTESIAN_POINT ( 'NONE',  ( -5.000000000000000000, 50.00000000000000000, -24.49489742783178059 ) ) ;
#6039 = CONICAL_SURFACE ( 'NONE', #6634, 5.035999999999999588, 0.7853981633974514986 ) ;
#6040 = CARTESIAN_POINT ( 'NONE',  ( 37.47500000054622404, 26.92701409722686634, 93.04388485072563242 ) ) ;
#6041 = CARTESIAN_POINT ( 'NONE',  ( 10.40000000000000036, 0.000000000000000000, 0.000000000000000000 ) ) ;
#6042 = ADVANCED_FACE ( 'NONE', ( #9528 ), #8629, .F. ) ;
#6043 = CARTESIAN_POINT ( 'NONE',  ( -4.338105965527106811, 47.49259679719147442, -27.66250853831607515 ) ) ;
#6044 = CARTESIAN_POINT ( 'NONE',  ( 39.37500000054622262, 27.65831843345427998, 90.79316153445363113 ) ) ;
#6045 = CARTESIAN_POINT ( 'NONE',  ( 39.89999999999999858, 22.43689772174679575, 98.29316153445363113 ) ) ;
#6046 = CARTESIAN_POINT ( 'NONE',  ( -6.610481451048220158, 27.51047402958706201, -24.11159121895188306 ) ) ;
#6047 = CARTESIAN_POINT ( 'NONE',  ( 45.97500000054623115, 15.71886984736413417, 96.68563167572563088 ) ) ;
#6048 = ORIENTED_EDGE ( 'NONE', *, *, #12350, .F. ) ;
#6049 = EDGE_CURVE ( 'NONE', #7736, #5467, #11036, .T. ) ;
#6050 = CARTESIAN_POINT ( 'NONE',  ( 29.55000000109246727, 22.43689772174679575, 98.29316153445363113 ) ) ;
#6051 = CARTESIAN_POINT ( 'NONE',  ( -1.325835098444672733, 10.08270123135439711, 24.96701611100131402 ) ) ;
#6052 = VERTEX_POINT ( 'NONE', #2985 ) ;
#6053 = CARTESIAN_POINT ( 'NONE',  ( 0.3314803829344796782, 55.00000000000000000, -21.00000000000000000 ) ) ;
#6054 = ORIENTED_EDGE ( 'NONE', *, *, #3099, .F. ) ;
#6055 = CARTESIAN_POINT ( 'NONE',  ( 6.614707539609227638, 12.47232065379156118, 27.21157843939673171 ) ) ;
#6056 = DIRECTION ( 'NONE',  ( 0.000000000000000000, 0.000000000000000000, 1.000000000000000000 ) ) ;
#6057 = DIRECTION ( 'NONE',  ( -1.000000000000000000, -0.000000000000000000, -0.000000000000000000 ) ) ;
#6058 = MANIFOLD_SOLID_BREP ( 'Thread1', #8096 ) ;
#6059=STYLED_ITEM('',(#12591),#6265);
#6060 = CARTESIAN_POINT ( 'NONE',  ( 30.37500000054622973, 13.07298590277314432, 88.54243821818161564 ) ) ;
#6061 = CARTESIAN_POINT ( 'NONE',  ( 33.37500000054621552, 27.65831843345427998, 90.79316153445363113 ) ) ;
#6062 = CARTESIAN_POINT ( 'NONE',  ( -4.493707279255195530, 52.21668117324033176, 27.63734306083194880 ) ) ;
#6063 = CLOSED_SHELL ( 'NONE', ( #11041, #9772, #7585, #3105, #5361, #10436, #4202, #3783 ) ) ;
#6064 = CARTESIAN_POINT ( 'NONE',  ( 43.65000000109246514, 20.00000000000000355, 98.29316153445363113 ) ) ;
#6065 = DIRECTION ( 'NONE',  ( 0.000000000000000000, 0.000000000000000000, 1.000000000000000000 ) ) ;
#6066 = VERTEX_POINT ( 'NONE', #11547 ) ;
#6067 = CARTESIAN_POINT ( 'NONE',  ( 47.97500000054622404, 17.63344945572769973, 98.07665518445361386 ) ) ;
#6068 = EDGE_CURVE ( 'NONE', #12402, #1690, #6851, .T. ) ;
#6069 = CARTESIAN_POINT ( 'NONE',  ( 1.302929565828678582, 54.83844695853547790, -24.96811105270434439 ) ) ;
#6070 = VERTEX_POINT ( 'NONE', #2858 ) ;
#6071 = DIRECTION ( 'NONE',  ( -1.000000000000000000, -0.000000000000000000, -0.000000000000000000 ) ) ;
#6072 = ORIENTED_EDGE ( 'NONE', *, *, #1496, .F. ) ;
#6073 = AXIS2_PLACEMENT_3D ( 'NONE', #8312, #8681, #8557 ) ;
#6074 = CARTESIAN_POINT ( 'NONE',  ( 10.00000000000000178, 0.000000000000000000, 8.000000000000000000 ) ) ;
#6075 = CARTESIAN_POINT ( 'NONE',  ( -9.917336477930691174, 18.67442475474294028, -22.94880690262607459 ) ) ;
#6076 = EDGE_CURVE ( 'NONE', #9736, #3312, #4146, .T. ) ;
#6077 = EDGE_CURVE ( 'NONE', #4797, #6345, #5258, .T. ) ;
#6078 = EDGE_CURVE ( 'NONE', #11262, #11877, #8514, .T. ) ;
#6079 = DIRECTION ( 'NONE',  ( 0.000000000000000000, 0.000000000000000000, -1.000000000000000000 ) ) ;
#6080 = LINE ( 'NONE', #2967, #7235 ) ;
#6081 = CARTESIAN_POINT ( 'NONE',  ( 7.723680589930663309, 26.35394802911231693, 86.80164316431257987 ) ) ;
#6082 = DIRECTION ( 'NONE',  ( 0.000000000000000000, 0.000000000000000000, -1.000000000000000000 ) ) ;
#6083 = CARTESIAN_POINT ( 'NONE',  ( 6.619094116331253552, 27.52385718499909117, 19.93550969653868066 ) ) ;
#6084 = CARTESIAN_POINT ( 'NONE',  ( -5.000000000000000000, 50.00000000000000000, 20.39607805437114152 ) ) ;
#6085 = CARTESIAN_POINT ( 'NONE',  ( -4.999999999999999112, 49.67329211228921082, 27.54995462791181993 ) ) ;
#6086 = CARTESIAN_POINT ( 'NONE',  ( 41.37500000054622262, 26.92701409722686634, 93.04388485072563242 ) ) ;
#6087 = DIRECTION ( 'NONE',  ( -1.000000000000000000, -0.000000000000000000, -0.000000000000000000 ) ) ;
#6088 = ORIENTED_EDGE ( 'NONE', *, *, #7443, .T. ) ;
#6089 = CARTESIAN_POINT ( 'NONE',  ( -7.935173117706110446, 13.90589240354496248, -26.85291110300881101 ) ) ;
#6090 = AXIS2_PLACEMENT_3D ( 'NONE', #11368, #2611, #831 ) ;
#6091 = CARTESIAN_POINT ( 'NONE',  ( 46.99999999999998579, 20.00000000000000355, 83.29316153445364534 ) ) ;
#6092 = CARTESIAN_POINT ( 'NONE',  ( 44.87500000054622973, 20.00000000000000355, 83.50966788445364841 ) ) ;
#6093 = CARTESIAN_POINT ( 'NONE',  ( 33.97500000054623115, 15.71886984736413417, 96.68563167572563088 ) ) ;
#6094 = CARTESIAN_POINT ( 'NONE',  ( 20.67500000054622689, 15.71886984736413773, 84.90069139318163138 ) ) ;
#6095 = CARTESIAN_POINT ( 'NONE',  ( 26.39999999999998792, 12.86707612778636012, 93.11078899226572503 ) ) ;
#6096 = FILL_AREA_STYLE ('',( #8063 ) ) ;
#6097 = CARTESIAN_POINT ( 'NONE',  ( 24.67500000054622689, 17.63344945572770328, 83.50966788445364841 ) ) ;
#6098 = ORIENTED_EDGE ( 'NONE', *, *, #10591, .T. ) ;
#6099 = PRODUCT ( 'socket head cap screw_iso_ISO 4762 M12 x 110 - 36N', 'socket head cap screw_iso_ISO 4762 M12 x 110 - 36N', '', ( #9833 ) ) ;
#6100 = CARTESIAN_POINT ( 'NONE',  ( 22.65000000109246514, 20.00000000000000355, 83.29316153445364534 ) ) ;
#6101 = ORIENTED_EDGE ( 'NONE', *, *, #5410, .F. ) ;
#6102 = ORIENTED_EDGE ( 'NONE', *, *, #11189, .F. ) ;
#6103 = DIRECTION ( 'NONE',  ( 0.000000000000000000, -0.4999999999999985012, 0.8660254037844394848 ) ) ;
#6104 = VERTEX_POINT ( 'NONE', #3106 ) ;
#6105 = CARTESIAN_POINT ( 'NONE',  ( -4.493909509445460415, 52.21603442804438799, -24.59310644668742540 ) ) ;
#6106 = AXIS2_PLACEMENT_3D ( 'NONE', #4063, #6036, #9910 ) ;
#6107 = CARTESIAN_POINT ( 'NONE',  ( 39.17500000054621978, 26.19570976099943849, 86.29171490190961435 ) ) ;
#6108 = CARTESIAN_POINT ( 'NONE',  ( -2.220456136781088219, 54.49171428740054068, -27.91344310064364009 ) ) ;
#6109 = CARTESIAN_POINT ( 'NONE',  ( 20.05000000109246372, 12.86707612778636012, 93.11078899226572503 ) ) ;
#6110 = CARTESIAN_POINT ( 'NONE',  ( 41.39999999999999147, 27.13292387221364876, 88.47553407664153724 ) ) ;
#6111 = EDGE_CURVE ( 'NONE', #1723, #378, #1086, .T. ) ;
#6112 = CARTESIAN_POINT ( 'NONE',  ( 48.37500000054622973, 13.07298590277314432, 88.54243821818161564 ) ) ;
#6113 = VERTEX_POINT ( 'NONE', #4952 ) ;
#6114 = CARTESIAN_POINT ( 'NONE',  ( 23.25000000109246656, 27.13292387221364876, 93.11078899226573924 ) ) ;
#6115 = CARTESIAN_POINT ( 'NONE',  ( -3.768871583585197360, 46.69794849765531808, 24.71539284385418611 ) ) ;
#6116 = ORIENTED_EDGE ( 'NONE', *, *, #145, .F. ) ;
#6117 = CARTESIAN_POINT ( 'NONE',  ( 4.339277897004357953, 52.50559309311499590, -20.54763125150147829 ) ) ;
#6118 = VERTEX_POINT ( 'NONE', #4251 ) ;
#6119 = B_SPLINE_CURVE_WITH_KNOTS ( 'NONE', 3,
 ( #3465, #6441, #7140, #5375, #3520, #611, #4477, #8104, #11017, #11140, #10305, #8167, #550, #4412, #8289, #1565, #7329, #9182, #1621, #8228, #9058, #11972, #489, #7267, #369, #4232 ),
 .UNSPECIFIED., .F., .F.,
 ( 4, 2, 2, 2, 2, 2, 2, 2, 2, 2, 2, 2, 4 ),
 ( 0.03159890529972236156, 0.03258580175252957789, 0.03357269820533679422, 0.03554649111095121994, 0.03653338756375844321, 0.03752028401656565260, 0.03949407692218008525, 0.04146786982779451791, 0.04245476628060172730, 0.04344166273340894363, 0.04541545563902336935, 0.04640235209183058568, 0.04738924854463780201 ),
 .UNSPECIFIED. ) ;
#6120 = CARTESIAN_POINT ( 'NONE',  ( -2.000000000000015543, 20.00000000000000355, 83.29316153445364534 ) ) ;
#6121 = CARTESIAN_POINT ( 'NONE',  ( 41.65000000109246514, 20.00000000000000355, 98.29316153445363113 ) ) ;
#6122 = SHAPE_REPRESENTATION ( 'socket head cap screw_iso_ISO 4762 M10 x 80 - 32N', ( #9021 ), #6962 ) ;
#6123 = CARTESIAN_POINT ( 'NONE',  ( 48.89999999999998437, 17.56310227825320069, 83.29316153445363113 ) ) ;
#6124 = PRODUCT_DEFINITION_CONTEXT ( 'detailed design', #12179, 'design' ) ;
#6125 = CARTESIAN_POINT ( 'NONE',  ( 30.87500000054622618, 22.36655054427230382, 83.50966788445364841 ) ) ;
#6126 = CARTESIAN_POINT ( 'NONE',  ( 33.97500000054620983, 17.63344945572769973, 98.07665518445361386 ) ) ;
#6127 = CARTESIAN_POINT ( 'NONE',  ( 3.429011037612589670E-15, 0.000000000000000000, 28.00000000000000355 ) ) ;
#6128 = CARTESIAN_POINT ( 'NONE',  ( 2.290457103807213457, 29.73981914200485477, 24.89699738223682246 ) ) ;
#6129 = FACE_OUTER_BOUND ( 'NONE', #4612, .T. ) ;
#6130 = EDGE_LOOP ( 'NONE', ( #389, #11583 ) ) ;
#6131 = CARTESIAN_POINT ( 'NONE',  ( 44.05000000109246372, 12.86707612778636012, 93.11078899226572503 ) ) ;
#6132 = ORIENTED_EDGE ( 'NONE', *, *, #1167, .T. ) ;
#6133 = CARTESIAN_POINT ( 'NONE',  ( -36.00000000000001421, 77.00000000000000000, 154.3533255156881978 ) ) ;
#6134 = EDGE_CURVE ( 'NONE', #3276, #5557, #264, .T. ) ;
#6135 = EDGE_LOOP ( 'NONE', ( #10232, #6661, #12396, #4924, #3828, #5632 ) ) ;
#6136 = CARTESIAN_POINT ( 'NONE',  ( -1.319698576403261825, 10.06506897208606333, -20.96877090753543627 ) ) ;
#6137 = LINE ( 'NONE', #5190, #5205 ) ;
#6138 = FACE_BOUND ( 'NONE', #6006, .T. ) ;
#6139 = CARTESIAN_POINT ( 'NONE',  ( 9.989732752402098015, 20.52140336093278350, 83.30683545822255098 ) ) ;
#6140 = LINE ( 'NONE', #3341, #11120 ) ;
#6141 = CARTESIAN_POINT ( 'NONE',  ( 1.321325188649778548, 29.91787852503522771, 20.96099891843594065 ) ) ;
#6142 = CARTESIAN_POINT ( 'NONE',  ( -0.1649528864959406427, 55.00000000000000000, 21.00000000000000355 ) ) ;
#6143 = CARTESIAN_POINT ( 'NONE',  ( -1.765688943715743031, 45.31926316749526507, 27.94468539932264406 ) ) ;
#6144 = ADVANCED_FACE ( 'NONE', ( #3175 ), #5965, .F. ) ;
#6145 = CARTESIAN_POINT ( 'NONE',  ( 43.07500000054622546, 26.19570976099943493, 86.29171490190961435 ) ) ;
#6146 = AXIS2_PLACEMENT_3D ( 'NONE', #8009, #10859, #7048 ) ;
#6147 = CARTESIAN_POINT ( 'NONE',  ( -4.967147891453746134, 49.34082981697670078, -24.50166768924217564 ) ) ;
#6148 = ORIENTED_EDGE ( 'NONE', *, *, #612, .T. ) ;
#6149 = CARTESIAN_POINT ( 'NONE',  ( -0.6582364880112170358, 54.96720335004231828, 24.99338302292539638 ) ) ;
#6150 = EDGE_CURVE ( 'NONE', #3840, #2709, #2286, .T. ) ;
#6151 = CARTESIAN_POINT ( 'NONE',  ( 4.491430111798321967, 52.22103771687890372, 24.59356092490497758 ) ) ;
#6152 = CARTESIAN_POINT ( 'NONE',  ( 46.07500000054622546, 15.71886984736413417, 96.68563167572563088 ) ) ;
#6153 = AXIS2_PLACEMENT_3D ( 'NONE', #677, #3589, #4732 ) ;
#6154 = CARTESIAN_POINT ( 'NONE',  ( 31.37500000054622973, 26.92701409722686634, 93.04388485072563242 ) ) ;
#6155 = CARTESIAN_POINT ( 'NONE',  ( 24.07500000054622546, 15.71886984736413417, 96.68563167572563088 ) ) ;
#6156 = LINE ( 'NONE', #8062, #4812 ) ;
#6157 = CARTESIAN_POINT ( 'NONE',  ( 6.000000000000000000, 5.839897972853064445, -8.673617379884035472E-15 ) ) ;
#6158 = CARTESIAN_POINT ( 'NONE',  ( 27.67500000054623044, 22.36655054427230027, 98.07665518445361386 ) ) ;
#6159 = VERTEX_POINT ( 'NONE', #5016 ) ;
#6160 = CARTESIAN_POINT ( 'NONE',  ( 33.05000000109247082, 27.13292387221364876, 88.47553407664153724 ) ) ;
#6161 = ORIENTED_EDGE ( 'NONE', *, *, #10279, .F. ) ;
#6162 = ORIENTED_EDGE ( 'NONE', *, *, #11334, .T. ) ;
#6163 = FACE_OUTER_BOUND ( 'NONE', #5942, .T. ) ;
#6164 = ORIENTED_EDGE ( 'NONE', *, *, #8928, .F. ) ;
#6165 = AXIS2_PLACEMENT_3D ( 'NONE', #8779, #1182, #4918 ) ;
#6166 = CARTESIAN_POINT ( 'NONE',  ( 0.000000000000000000, 0.000000000000000000, 0.000000000000000000 ) ) ;
#6167 = CIRCLE ( 'NONE', #10216, 5.999999999999999112 ) ;
#6168 = CARTESIAN_POINT ( 'NONE',  ( 36.57500000054621125, 13.80429023900056684, 86.29171490190961435 ) ) ;
#6169 = CARTESIAN_POINT ( 'NONE',  ( -6.999999999999978684, 20.00000000000000355, 109.9999999999999858 ) ) ;
#6170 = CARTESIAN_POINT ( 'NONE',  ( 38.79999999999999005, 15.59161060780646046, 84.72553407664153724 ) ) ;
#6171 = CARTESIAN_POINT ( 'NONE',  ( 44.87500000054623683, 22.36655054427230382, 83.50966788445364841 ) ) ;
#6172 = ORIENTED_EDGE ( 'NONE', *, *, #67, .F. ) ;
#6173 = AXIS2_PLACEMENT_3D ( 'NONE', #7250, #3448, #7313 ) ;
#6174 = CARTESIAN_POINT ( 'NONE',  ( 22.15000000109246869, 12.11403331821300533, 90.79316153445363113 ) ) ;
#6175 = DIRECTION ( 'NONE',  ( 1.000000000000000000, 0.000000000000000000, 0.000000000000000000 ) ) ;
#6176 = VERTEX_POINT ( 'NONE', #8815 ) ;
#6177 = CARTESIAN_POINT ( 'NONE',  ( -9.483329012715213224, 23.23888378086489581, 26.34647234298155993 ) ) ;
#6178 = ORIENTED_EDGE ( 'NONE', *, *, #175, .T. ) ;
#6179 = CARTESIAN_POINT ( 'NONE',  ( 2.608216138242892335, 10.34052515137489969, 27.88005196315802792 ) ) ;
#6180 = CARTESIAN_POINT ( 'NONE',  ( 40.75000000109245946, 22.43689772174679575, 83.29316153445363113 ) ) ;
#6181 = ADVANCED_FACE ( 'NONE', ( #10979 ), #10032, .T. ) ;
#6182 = AXIS2_PLACEMENT_3D ( 'NONE', #12530, #3838, #11580 ) ;
#6183 = CARTESIAN_POINT ( 'NONE',  ( -6.999999999999999112, 40.00000000000000000, 69.99999999999998579 ) ) ;
#6184 = CARTESIAN_POINT ( 'NONE',  ( 27.87500000054622618, 17.63344945572769973, 98.07665518445361386 ) ) ;
#6185 = CARTESIAN_POINT ( 'NONE',  ( 30.67500000054622333, 15.71886984736413773, 84.90069139318163138 ) ) ;
#6186 = CARTESIAN_POINT ( 'NONE',  ( 5.018622449780372641, 28.67437547244667684, 27.55219550168085263 ) ) ;
#6187 = CARTESIAN_POINT ( 'NONE',  ( 22.35000000109246443, 13.62011893735970958, 86.15790661882942914 ) ) ;
#6188 = ORIENTED_EDGE ( 'NONE', *, *, #4944, .F. ) ;
#6189 = CARTESIAN_POINT ( 'NONE',  ( 43.35000000109246088, 26.37988106264029398, 95.42841645007781892 ) ) ;
#6190 = ORIENTED_EDGE ( 'NONE', *, *, #8359, .T. ) ;
#6191 = CARTESIAN_POINT ( 'NONE',  ( 0.000000000000000000, -2.342598717236902051, 4.057500000000004547 ) ) ;
#6192 = CIRCLE ( 'NONE', #1509, 8.400000000000000355 ) ;
#6193 = ORIENTED_EDGE ( 'NONE', *, *, #10958, .F. ) ;
#6194 = CARTESIAN_POINT ( 'NONE',  ( -0.6576044892141179599, 10.01619439626406383, -24.99350884773162207 ) ) ;
#6195 = CARTESIAN_POINT ( 'NONE',  ( -7.300087775502666965, 26.84214942138161675, 23.91163959704068631 ) ) ;
#6196 = LINE ( 'NONE', #10192, #5944 ) ;
#6197 = AXIS2_PLACEMENT_3D ( 'NONE', #11340, #11273, #3345 ) ;
#6198 = SURFACE_STYLE_FILL_AREA ( #5316 ) ;
#6199 = PRODUCT_DEFINITION_SHAPE ( 'NONE', 'NONE',  #12549 ) ;
#6200 = ADVANCED_FACE ( 'NONE', ( #1341 ), #387, .F. ) ;
#6201 = AXIS2_PLACEMENT_3D ( 'NONE', #7016, #7076, #2129 ) ;
#6202 = CARTESIAN_POINT ( 'NONE',  ( -6.106142575418606278, 12.07400325324896784, 24.24423224237354901 ) ) ;
#6203 = DIRECTION ( 'NONE',  ( -1.000000000000000000, -0.000000000000000000, -0.000000000000000000 ) ) ;
#6204 = CARTESIAN_POINT ( 'NONE',  ( -10.00000000000000355, 20.00000000000000355, 18.46618531261938756 ) ) ;
#6205 = DIRECTION ( 'NONE',  ( 0.000000000000000000, 0.000000000000000000, 1.000000000000000000 ) ) ;
#6206 = CARTESIAN_POINT ( 'NONE',  ( 3.429010155815331973E-15, 45.00000000000000711, 28.00000000000000355 ) ) ;
#6207 = EDGE_CURVE ( 'NONE', #11695, #527, #10121, .T. ) ;
#6208 = CARTESIAN_POINT ( 'NONE',  ( -1.612729787338046394, 45.25594143338945941, -24.94976830077123964 ) ) ;
#6209 = ORIENTED_EDGE ( 'NONE', *, *, #10552, .T. ) ;
#6210 = CARTESIAN_POINT ( 'NONE',  ( -4.556215257066872582, 52.06578128350423640, 24.58139409886873139 ) ) ;
#6211 = DIRECTION ( 'NONE',  ( 1.000000000000000000, -0.000000000000000000, -0.000000000000000000 ) ) ;
#6212 = CARTESIAN_POINT ( 'NONE',  ( 43.77500000054622120, 22.36655054427230027, 98.07665518445361386 ) ) ;
#6213 = AXIS2_PLACEMENT_3D ( 'NONE', #507, #9262, #6275 ) ;
#6214 = CARTESIAN_POINT ( 'NONE',  ( 25.47500000054622760, 26.19570976099943849, 95.29460816699764791 ) ) ;
#6215 = CARTESIAN_POINT ( 'NONE',  ( 7.617757055713122227, 13.51299916189778649, 86.99997826776774446 ) ) ;
#6216 = CARTESIAN_POINT ( 'NONE',  ( 11.99999999999999645, 0.000000000000000000, 0.000000000000000000 ) ) ;
#6217 = LINE ( 'NONE', #10091, #8300 ) ;
#6218 = CARTESIAN_POINT ( 'NONE',  ( 25.47500000054622760, 26.19570976099943493, 95.29460816699764791 ) ) ;
#6219 = ORIENTED_EDGE ( 'NONE', *, *, #10468, .T. ) ;
#6220 = EDGE_CURVE ( 'NONE', #1348, #8883, #7098, .T. ) ;
#6221 = DIRECTION ( 'NONE',  ( 0.000000000000000000, 0.000000000000000000, 1.000000000000000000 ) ) ;
#6222 = EDGE_LOOP ( 'NONE', ( #11236, #4868, #6358, #2326 ) ) ;
#6223 = CARTESIAN_POINT ( 'NONE',  ( 10.00000000000000355, 20.00000000000000355, 83.29316153445363113 ) ) ;
#6224 = VERTEX_POINT ( 'NONE', #134 ) ;
#6225 =( GEOMETRIC_REPRESENTATION_CONTEXT ( 3 ) GLOBAL_UNCERTAINTY_ASSIGNED_CONTEXT ( ( #7722 ) ) GLOBAL_UNIT_ASSIGNED_CONTEXT ( ( #5192, #11020, #5378 ) ) REPRESENTATION_CONTEXT ( 'NONE', 'WORKASPACE' ) );
#6226 = SHAPE_REPRESENTATION_RELATIONSHIP ( 'NONE' , 'NONE' ,  #6122, #11414 ) ;
#6227 = EDGE_CURVE ( 'NONE', #9270, #3052, #5083, .T. ) ;
#6228 = CARTESIAN_POINT ( 'NONE',  ( 34.37500000054621552, 12.34168156654572357, 90.79316153445363113 ) ) ;
#6229 = CARTESIAN_POINT ( 'NONE',  ( -111.8465843842649292, 69.50000000000000000, 101.8533255156881978 ) ) ;
#6230 = CARTESIAN_POINT ( 'NONE',  ( -2.501722953165860464, 45.66777005292055236, -27.88839186769926215 ) ) ;
#6231 = CARTESIAN_POINT ( 'NONE',  ( 34.67500000054622689, 15.71886984736413773, 84.90069139318163138 ) ) ;
#6232 = CARTESIAN_POINT ( 'NONE',  ( 35.69999999999997442, 26.37988106264029398, 95.42841645007781892 ) ) ;
#6233 = CIRCLE ( 'NONE', #4410, 13.85889894354065710 ) ;
#6234 = CARTESIAN_POINT ( 'NONE',  ( 44.77500000054623541, 20.00000000000000355, 83.50966788445364841 ) ) ;
#6235 = ORIENTED_EDGE ( 'NONE', *, *, #160, .F. ) ;
#6236 = CARTESIAN_POINT ( 'NONE',  ( 25.55000000109246372, 22.43689772174679575, 98.29316153445363113 ) ) ;
#6237 = CARTESIAN_POINT ( 'NONE',  ( -10.00000000000001066, 19.67111324348436696, 22.91287847477920536 ) ) ;
#6238 = ORIENTED_EDGE ( 'NONE', *, *, #4994, .F. ) ;
#6239 = DIRECTION ( 'NONE',  ( -0.000000000000000000, -0.000000000000000000, 1.000000000000000000 ) ) ;
#6240 = ORIENTED_EDGE ( 'NONE', *, *, #6546, .F. ) ;
#6241 = CARTESIAN_POINT ( 'NONE',  ( 21.35000000109246443, 26.37988106264029398, 95.42841645007781892 ) ) ;
#6242 = CARTESIAN_POINT ( 'NONE',  ( 0.000000000000000000, 0.000000000000000000, 0.000000000000000000 ) ) ;
#6243 = CARTESIAN_POINT ( 'NONE',  ( -27.49999999999999645, 20.00000000000000355, 170.0000119999999697 ) ) ;
#6244 = CARTESIAN_POINT ( 'NONE',  ( 33.17500000054622689, 26.92701409722686634, 88.54243821818162985 ) ) ;
#6245 = CARTESIAN_POINT ( 'NONE',  ( 24.47500000054622404, 13.07298590277314432, 88.54243821818161564 ) ) ;
#6246 = FACE_OUTER_BOUND ( 'NONE', #5085, .T. ) ;
#6247 = DIRECTION ( 'NONE',  ( 0.000000000000000000, 1.000000000000000000, 0.000000000000000000 ) ) ;
#6248 = AXIS2_PLACEMENT_3D ( 'NONE', #11318, #846, #5612 ) ;
#6249 = EDGE_LOOP ( 'NONE', ( #4466, #503, #4141, #8285 ) ) ;
#6250 = CARTESIAN_POINT ( 'NONE',  ( 43.25000000109246656, 27.13292387221364876, 93.11078899226573924 ) ) ;
#6251 = SURFACE_STYLE_FILL_AREA ( #5308 ) ;
#6252 = VERTEX_POINT ( 'NONE', #7871 ) ;
#6253 = FACE_OUTER_BOUND ( 'NONE', #2124, .T. ) ;
#6254=STYLED_ITEM('',(#12584),#2081);
#6255 = ORIENTED_EDGE ( 'NONE', *, *, #4509, .F. ) ;
#6256 = CARTESIAN_POINT ( 'NONE',  ( -9.983516779091171855, 19.33659569722678029, -22.92009366892111899 ) ) ;
#6257 = CARTESIAN_POINT ( 'NONE',  ( -8.123193803314322281, 25.84109844632562769, 23.64424386314666648 ) ) ;
#6258 =( BOUNDED_CURVE ( )  B_SPLINE_CURVE ( 2, ( #6965, #1891, #2912, #6843, #59, #6022, #2978, #3922, #3318, #3985, #10704 ),
 .UNSPECIFIED., .F., .F. ) 
 B_SPLINE_CURVE_WITH_KNOTS ( ( 3, 2, 2, 2, 2, 3 ),
 ( 0.4000000000000001332, 0.4066666666666667873, 0.4133333333333334414, 0.4200000000000000955, 0.4266666666666668051, 0.4333333333333334592 ),
 .UNSPECIFIED. ) 
 CURVE ( )  GEOMETRIC_REPRESENTATION_ITEM ( )  RATIONAL_B_SPLINE_CURVE ( ( 0.9999999999999992228, 0.9510565162951543083, 1.000000000000000000, 0.9510565162951535312, 1.000000000000000000, 0.9510565162951535312, 1.000000000000000000, 0.9510565162951535312, 1.000000000000000000, 0.9510565162951527540, 1.000000000000000888 ) ) 
 REPRESENTATION_ITEM ( '' )  );
#6259 = CIRCLE ( 'NONE', #6643, 7.499999999999978684 ) ;
#6260 = COLOUR_RGB ( '',0.7921568627450980005, 0.8196078431372548767, 0.9333333333333333481 ) ;
#6261 = CARTESIAN_POINT ( 'NONE',  ( 3.298734236876446957, 53.76100060739371145, 24.78173945428942204 ) ) ;
#6262 = CARTESIAN_POINT ( 'NONE',  ( -9.481487189274945493, 16.75591109918640242, 23.13382230614692148 ) ) ;
#6263 = CARTESIAN_POINT ( 'NONE',  ( -5.000000000000000000, 50.00000000000000000, -28.00000000000000711 ) ) ;
#6264 = DIRECTION ( 'NONE',  ( 0.000000000000000000, 0.4999999999999988898, -0.8660254037844392627 ) ) ;
#6265 = MANIFOLD_SOLID_BREP ( 'Hex', #4436 ) ;
#6266 = LINE ( 'NONE', #9254, #10008 ) ;
#6267 = ADVANCED_FACE ( 'NONE', ( #7290 ), #5148, .F. ) ;
#6268 = CARTESIAN_POINT ( 'NONE',  ( 6.611279324052055095, 27.53068265742442122, 24.11471400905219298 ) ) ;
#6269 = VECTOR ( 'NONE', #10913, 1000.000000000000000 ) ;
#6270 =( REPRESENTATION_RELATIONSHIP ('NONE','NONE', #4262, #6122 ) REPRESENTATION_RELATIONSHIP_WITH_TRANSFORMATION ( #10581 )SHAPE_REPRESENTATION_RELATIONSHIP( ) );
#6271 = CYLINDRICAL_SURFACE ( 'NONE', #425, 9.000000000000000000 ) ;
#6272 = ORIENTED_EDGE ( 'NONE', *, *, #2188, .F. ) ;
#6273 = CARTESIAN_POINT ( 'NONE',  ( -7.304238131681169754, 13.16224956375578081, -27.03155692136176214 ) ) ;
#6274 = CARTESIAN_POINT ( 'NONE',  ( 27.49999999999999645, 20.00000000000000355, 99.99999999999997158 ) ) ;
#6275 = DIRECTION ( 'NONE',  ( 0.000000000000000000, 0.000000000000000000, 1.000000000000000000 ) ) ;
#6276 = CARTESIAN_POINT ( 'NONE',  ( 43.87500000054622973, 20.00000000000000355, 98.07665518445361386 ) ) ;
#6277 = EDGE_CURVE ( 'NONE', #10865, #7736, #12333, .T. ) ;
#6278 = CARTESIAN_POINT ( 'NONE',  ( 24.27500000054622475, 12.34168156654572357, 90.79316153445363113 ) ) ;
#6279 = CARTESIAN_POINT ( 'NONE',  ( 9.482520708152488709, 16.75818430496380529, -23.13341755400983502 ) ) ;
#6280 = CARTESIAN_POINT ( 'NONE',  ( 27.49999999999999645, 20.00000000000000355, 172.0000000000000000 ) ) ;
#6281 = FACE_OUTER_BOUND ( 'NONE', #3580, .T. ) ;
#6282 = DIRECTION ( 'NONE',  ( 0.000000000000000000, 0.000000000000000000, -1.000000000000000000 ) ) ;
#6283 = ORIENTED_EDGE ( 'NONE', *, *, #4293, .T. ) ;
#6284 = DIRECTION ( 'NONE',  ( 1.000000000000000000, 0.000000000000000000, 0.000000000000000000 ) ) ;
#6285 = EDGE_LOOP ( 'NONE', ( #6054, #12478, #2676, #1661, #7264, #8513 ) ) ;
#6286 = VECTOR ( 'NONE', #11637, 1000.000000000000000 ) ;
#6287 = DIRECTION ( 'NONE',  ( 0.000000000000000000, -1.000000000000000000, 0.000000000000000000 ) ) ;
#6288 = ADVANCED_FACE ( 'NONE', ( #12120 ), #1583, .F. ) ;
#6289 = EDGE_LOOP ( 'NONE', ( #5957, #11835, #5106, #7017, #10949 ) ) ;
#6290 = ADVANCED_FACE ( 'NONE', ( #4434 ), #2592, .F. ) ;
#6291 = CARTESIAN_POINT ( 'NONE',  ( 31.37500000054622262, 27.65831843345427998, 90.79316153445363113 ) ) ;
#6292 = CARTESIAN_POINT ( 'NONE',  ( 0.000000000000000000, 139.9999999999999716, -21.00000000000000000 ) ) ;
#6293 = ADVANCED_FACE ( 'NONE', ( #4375 ), #5334, .F. ) ;
#6294 = CARTESIAN_POINT ( 'NONE',  ( 48.17500000054623399, 13.07298590277314254, 93.04388485072563242 ) ) ;
#6295 = CARTESIAN_POINT ( 'NONE',  ( 36.77500000054622831, 17.63344945572770328, 83.50966788445364841 ) ) ;
#6296 = CARTESIAN_POINT ( 'NONE',  ( 33.69999999999997442, 26.37988106264029398, 95.42841645007781892 ) ) ;
#6297 = AXIS2_PLACEMENT_3D ( 'NONE', #5644, #11473, #636 ) ;
#6298 = CARTESIAN_POINT ( 'NONE',  ( 46.77500000054622831, 20.00000000000000355, 83.50966788445364841 ) ) ;
#6299 = ORIENTED_EDGE ( 'NONE', *, *, #9469, .T. ) ;
#6300 = CARTESIAN_POINT ( 'NONE',  ( 23.85000000109246443, 15.59161060780645691, 96.86078899226572503 ) ) ;
#6301 = CARTESIAN_POINT ( 'NONE',  ( -5.845694806184612347, 11.88009017893230990, 24.30851799965319060 ) ) ;
#6302 = ORIENTED_EDGE ( 'NONE', *, *, #5312, .T. ) ;
#6303 = EDGE_CURVE ( 'NONE', #11952, #6721, #6217, .T. ) ;
#6304 = CARTESIAN_POINT ( 'NONE',  ( -8.968509794689500936, 24.43547164034384878, 26.52531781923291376 ) ) ;
#6305 = ORIENTED_EDGE ( 'NONE', *, *, #9707, .F. ) ;
#6306 = LINE ( 'NONE', #6367, #699 ) ;
#6307 = AXIS2_PLACEMENT_3D ( 'NONE', #7373, #5292, #1480 ) ;
#6308 = DIRECTION ( 'NONE',  ( 0.000000000000000000, 0.000000000000000000, -1.000000000000000000 ) ) ;
#6309 = CARTESIAN_POINT ( 'NONE',  ( 27.49999999999999645, 20.00000000000000355, 189.9999999999999716 ) ) ;
#6310 = DIRECTION ( 'NONE',  ( 1.000000000000000000, -0.000000000000000000, -0.000000000000000000 ) ) ;
#6311 = ADVANCED_FACE ( 'NONE', ( #10154 ), #4498, .T. ) ;
#6312 = CARTESIAN_POINT ( 'NONE',  ( 22.27500000054622475, 12.34168156654572535, 90.79316153445363113 ) ) ;
#6313 = CARTESIAN_POINT ( 'NONE',  ( 28.17500000054621978, 13.80429023900056507, 95.29460816699764791 ) ) ;
#6314 = CARTESIAN_POINT ( 'NONE',  ( 7.928997479961922501, 26.10222245235190641, 26.85474570151987450 ) ) ;
#6315 = DIRECTION ( 'NONE',  ( -1.000000000000000000, 0.000000000000000000, 0.000000000000000000 ) ) ;
#6316 = EDGE_LOOP ( 'NONE', ( #715, #3759, #7183, #1539 ) ) ;
#6317 = CARTESIAN_POINT ( 'NONE',  ( 44.45000000109246230, 15.59161060780646046, 84.72553407664153724 ) ) ;
#6318 = ORIENTED_EDGE ( 'NONE', *, *, #6668, .T. ) ;
#6319 = DIRECTION ( 'NONE',  ( -1.000000000000000000, -0.000000000000000000, -0.000000000000000000 ) ) ;
#6320 = EDGE_LOOP ( 'NONE', ( #4499, #8887, #10619, #89, #6219 ) ) ;
#6321 = DIRECTION ( 'NONE',  ( 1.000000000000000000, 0.000000000000000000, 0.000000000000000000 ) ) ;
#6322 = DIRECTION ( 'NONE',  ( -1.000000000000000000, -0.000000000000000000, -0.000000000000000000 ) ) ;
#6323 = CARTESIAN_POINT ( 'NONE',  ( 19.87500000054622973, 17.63344945572769973, 98.07665518445361386 ) ) ;
#6324 = CARTESIAN_POINT ( 'NONE',  ( -9.918789871757258680, 18.68607266337350836, 22.94817778295035993 ) ) ;
#6325 = CYLINDRICAL_SURFACE ( 'NONE', #10701, 7.499999999999978684 ) ;
#6326 = DIRECTION ( 'NONE',  ( 0.000000000000000000, -0.8660254037844392627, -0.4999999999999988898 ) ) ;
#6327 = CARTESIAN_POINT ( 'NONE',  ( -7.533400678184611898, 13.39129849816836249, 26.97176181097763958 ) ) ;
#6328 = CARTESIAN_POINT ( 'NONE',  ( 4.149575074854375600, 29.10425525072577102, 24.65509887497819008 ) ) ;
#6329 = CARTESIAN_POINT ( 'NONE',  ( 23.99999999999998579, 20.00000000000000355, 98.29316153445363113 ) ) ;
#6330 = ORIENTED_EDGE ( 'NONE', *, *, #4009, .F. ) ;
#6331 =( BOUNDED_CURVE ( )  B_SPLINE_CURVE ( 3, ( #9764, #3981, #7858, #880 ),
 .UNSPECIFIED., .F., .F. ) 
 B_SPLINE_CURVE_WITH_KNOTS ( ( 4, 4 ),
 ( 4.712388980384689674, 6.283185307179586232 ),
 .UNSPECIFIED. ) 
 CURVE ( )  GEOMETRIC_REPRESENTATION_ITEM ( )  RATIONAL_B_SPLINE_CURVE ( ( 1.000000000000000000, 0.8047378541243649375, 0.8047378541243649375, 1.000000000000000000 ) ) 
 REPRESENTATION_ITEM ( '' )  );
#6332 = B_SPLINE_CURVE_WITH_KNOTS ( 'NONE', 3,
 ( #7246, #9223, #5351, #5414, #2424, #529, #4389, #12136, #10996, #2484, #2248, #6115, #11059, #8267, #7122, #3255, #5290, #7182, #4454, #2306 ),
 .UNSPECIFIED., .F., .F.,
 ( 4, 2, 2, 2, 2, 2, 2, 2, 2, 4 ),
 ( 0.007837842730401771429, 0.008817088216258357411, 0.009796333702114945127, 0.01028595644504323552, 0.01077557918797152590, 0.01175482467382810668, 0.01273407015968468919, 0.01371331564554126997, 0.01469256113139785075, 0.01567180661725443153 ),
 .UNSPECIFIED. ) ;
#6333 = CARTESIAN_POINT ( 'NONE',  ( 1.614504882520976681, 45.25664461204844713, 24.94963714481321304 ) ) ;
#6334 = ADVANCED_FACE ( 'NONE', ( #6465 ), #8189, .F. ) ;
#6335 = CARTESIAN_POINT ( 'NONE',  ( 2.217963917954424602, 54.49304390046189894, 24.90325875173717662 ) ) ;
#6336 = CARTESIAN_POINT ( 'NONE',  ( 43.67500000054621978, 24.28113015263587116, 96.68563167572563088 ) ) ;
#6337 = CARTESIAN_POINT ( 'NONE',  ( 28.37500000054622618, 13.07298590277314432, 88.54243821818161564 ) ) ;
#6338 = DIRECTION ( 'NONE',  ( 0.000000000000000000, -1.000000000000000000, 0.000000000000000000 ) ) ;
#6339 = CARTESIAN_POINT ( 'NONE',  ( -111.8465843842649292, 84.49999999999998579, 146.8533255156881978 ) ) ;
#6340 = AXIS2_PLACEMENT_3D ( 'NONE', #5961, #9837, #491 ) ;
#6341 = FACE_OUTER_BOUND ( 'NONE', #847, .T. ) ;
#6342 = LINE ( 'NONE', #569, #7065 ) ;
#6343 = EDGE_LOOP ( 'NONE', ( #4599, #1956, #9552, #5231 ) ) ;
#6344 = DIRECTION ( 'NONE',  ( 0.000000000000000000, 0.000000000000000000, -1.000000000000000000 ) ) ;
#6345 = VERTEX_POINT ( 'NONE', #5523 ) ;
#6346 = CARTESIAN_POINT ( 'NONE',  ( 0.000000000000000000, -2.919948986426523341, 5.057500000000002771 ) ) ;
#6347 = ORIENTED_EDGE ( 'NONE', *, *, #1089, .T. ) ;
#6348 =( NAMED_UNIT ( * ) SI_UNIT ( $, .STERADIAN. ) SOLID_ANGLE_UNIT ( ) );
#6349 = CIRCLE ( 'NONE', #478, 6.000000000000003553 ) ;
#6350 = CARTESIAN_POINT ( 'NONE',  ( 35.07500000054622546, 24.28113015263587471, 84.90069139318163138 ) ) ;
#6351 = CARTESIAN_POINT ( 'NONE',  ( -4.840361584771153858, 51.29513118448893749, -27.57852565106875886 ) ) ;
#6352 = CARTESIAN_POINT ( 'NONE',  ( 45.77500000054622831, 20.00000000000000355, 98.07665518445361386 ) ) ;
#6353 = CARTESIAN_POINT ( 'NONE',  ( 34.77500000054622831, 17.63344945572770328, 83.50966788445364841 ) ) ;
#6354 = CARTESIAN_POINT ( 'NONE',  ( 34.39999999999998437, 12.86707612778636012, 93.11078899226572503 ) ) ;
#6355 = EDGE_CURVE ( 'NONE', #7325, #10212, #3328, .T. ) ;
#6356 = CARTESIAN_POINT ( 'NONE',  ( 9.737811142203947057, 22.29842083447240597, 23.02563804066124931 ) ) ;
#6357 = CARTESIAN_POINT ( 'NONE',  ( 41.97500000054623115, 15.71886984736413417, 96.68563167572563088 ) ) ;
#6358 = ORIENTED_EDGE ( 'NONE', *, *, #6077, .F. ) ;
#6359 = VECTOR ( 'NONE', #5806, 1000.000000000000000 ) ;
#6360 = CARTESIAN_POINT ( 'NONE',  ( 26.35000000109246443, 13.62011893735971135, 86.15790661882942914 ) ) ;
#6361 = CARTESIAN_POINT ( 'NONE',  ( -10.00000000000000355, 20.00000000000000355, 22.91287847477919826 ) ) ;
#6362 = ORIENTED_EDGE ( 'NONE', *, *, #9800, .F. ) ;
#6363 = CARTESIAN_POINT ( 'NONE',  ( 6.000000000000000000, 2.919948986426538884, 5.057499999999996554 ) ) ;
#6364 = PRODUCT_DEFINITION_FORMATION_WITH_SPECIFIED_SOURCE ( 'ANY', '', #5783, .NOT_KNOWN. ) ;
#6365 = EDGE_CURVE ( 'NONE', #9622, #2202, #9308, .T. ) ;
#6366 = EDGE_LOOP ( 'NONE', ( #3427, #4897, #3364, #7810, #8268, #4404 ) ) ;
#6367 = CARTESIAN_POINT ( 'NONE',  ( 6.000000000000000000, 2.919948986426540660, 5.057499999999996554 ) ) ;
#6368 = CARTESIAN_POINT ( 'NONE',  ( 21.15000000109246514, 27.88596668178699645, 90.79316153445363113 ) ) ;
#6369 = CARTESIAN_POINT ( 'NONE',  ( 34.72841614740047333, 18.00000000000000355, 170.0000119999999697 ) ) ;
#6370 = CARTESIAN_POINT ( 'NONE',  ( 32.45000000109246940, 15.59161060780646046, 84.72553407664153724 ) ) ;
#6371 = CARTESIAN_POINT ( 'NONE',  ( 21.57500000054622546, 24.28113015263587116, 96.68563167572563088 ) ) ;
#6372 = CARTESIAN_POINT ( 'NONE',  ( 26.37500000054622618, 12.34168156654572535, 90.79316153445363113 ) ) ;
#6373 = VECTOR ( 'NONE', #2377, 1000.000000000000000 ) ;
#6374 = CARTESIAN_POINT ( 'NONE',  ( 6.610911640192685290, 27.53087490925221559, 27.21248546868482876 ) ) ;
#6375 = DIRECTION ( 'NONE',  ( 1.000000000000000000, -0.000000000000000000, -0.000000000000000000 ) ) ;
#6376 = EDGE_LOOP ( 'NONE', ( #11074, #4869, #6164 ) ) ;
#6377 = CARTESIAN_POINT ( 'NONE',  ( 43.65000000109246514, 20.00000000000000355, 98.29316153445363113 ) ) ;
#6378 = ORIENTED_EDGE ( 'NONE', *, *, #9618, .T. ) ;
#6379 = CARTESIAN_POINT ( 'NONE',  ( 6.000000000000000000, -2.919948986426523341, 5.057500000000002771 ) ) ;
#6380 = EDGE_CURVE ( 'NONE', #5465, #12457, #6342, .T. ) ;
#6381 = ORIENTED_EDGE ( 'NONE', *, *, #1939, .F. ) ;
#6382 = AXIS2_PLACEMENT_3D ( 'NONE', #5319, #6754, #12349 ) ;
#6383 = CARTESIAN_POINT ( 'NONE',  ( 2.505765861943965334, 54.33918026639940990, 20.85177847850087574 ) ) ;
#6384 = CARTESIAN_POINT ( 'NONE',  ( -7.930305867179300527, 26.10041404063223780, 23.70984975861344779 ) ) ;
#6385 = ADVANCED_FACE ( 'NONE', ( #1520 ), #9269, .F. ) ;
#6386 = CARTESIAN_POINT ( 'NONE',  ( -0.6638428588095105498, 10.01651532611708895, 24.99338002059894137 ) ) ;
#6387 = CARTESIAN_POINT ( 'NONE',  ( 5.000000000000000000, 4.685197434473814759, -5.637851296924623057E-15 ) ) ;
#6388 = CIRCLE ( 'NONE', #5186, 9.000000000000000000 ) ;
#6389 = CARTESIAN_POINT ( 'NONE',  ( 41.99999999999998579, 20.00000000000000355, 98.29316153445363113 ) ) ;
#6390 = CARTESIAN_POINT ( 'NONE',  ( 0.000000000000000000, 50.00000000000000000, -28.00000000000000711 ) ) ;
#6391 = DIRECTION ( 'NONE',  ( 1.000000000000000000, 0.000000000000000000, 0.000000000000000000 ) ) ;
#6392 = CARTESIAN_POINT ( 'NONE',  ( 27.49999999999999645, 20.00000000000000355, 169.9999999999999716 ) ) ;
#6393 = ORIENTED_EDGE ( 'NONE', *, *, #9543, .F. ) ;
#6394 = AXIS2_PLACEMENT_3D ( 'NONE', #334, #2097, #1224 ) ;
#6395 = DIRECTION ( 'NONE',  ( 1.000000000000000000, -0.000000000000000000, -0.000000000000000000 ) ) ;
#6396 = CARTESIAN_POINT ( 'NONE',  ( 28.79999999999999005, 15.59161060780646046, 84.72553407664153724 ) ) ;
#6397 = CARTESIAN_POINT ( 'NONE',  ( 36.17500000054623399, 13.80429023900056507, 95.29460816699764791 ) ) ;
#6398 = CARTESIAN_POINT ( 'NONE',  ( 25.87500000054622618, 17.63344945572769973, 98.07665518445361386 ) ) ;
#6399 = CARTESIAN_POINT ( 'NONE',  ( 9.105349949761121664, 15.85277269881838258, -23.28327519851026040 ) ) ;
#6400 = CARTESIAN_POINT ( 'NONE',  ( 21.65000000109246514, 20.00000000000000355, 98.29316153445363113 ) ) ;
#6401 = CYLINDRICAL_SURFACE ( 'NONE', #9818, 7.499999999999992895 ) ;
#6402 = CARTESIAN_POINT ( 'NONE',  ( 31.19999999999998863, 24.40838939219355197, 84.72553407664153724 ) ) ;
#6403 =( BOUNDED_CURVE ( )  B_SPLINE_CURVE ( 2, ( #2273, #8234, #1323, #5194, #9062, #1385, #5254, #1449, #3525, #11515, #5692 ),
 .UNSPECIFIED., .F., .F. ) 
 B_SPLINE_CURVE_WITH_KNOTS ( ( 3, 2, 2, 2, 2, 3 ),
 ( 0.9000000000000000222, 0.9066666666666666208, 0.9133333333333333304, 0.9200000000000000400, 0.9266666666666666385, 0.9333333333333333481 ),
 .UNSPECIFIED. ) 
 CURVE ( )  GEOMETRIC_REPRESENTATION_ITEM ( )  RATIONAL_B_SPLINE_CURVE ( ( 1.000000000000000000, 0.9510565162951535312, 1.000000000000000000, 0.9510565162951535312, 1.000000000000000000, 0.9510565162951535312, 1.000000000000000000, 0.9510565162951535312, 1.000000000000000000, 0.9510565162951535312, 1.000000000000000000 ) ) 
 REPRESENTATION_ITEM ( '' )  );
#6404 = VERTEX_POINT ( 'NONE', #12426 ) ;
#6405 = DIRECTION ( 'NONE',  ( 0.000000000000000000, 0.000000000000000000, 1.000000000000000000 ) ) ;
#6406 = ORIENTED_EDGE ( 'NONE', *, *, #7973, .F. ) ;
#6407 = ADVANCED_FACE ( 'NONE', ( #2908 ), #9515, .T. ) ;
#6408 = DIRECTION ( 'NONE',  ( -0.000000000000000000, -0.000000000000000000, 1.000000000000000000 ) ) ;
#6409 = DIRECTION ( 'NONE',  ( -1.000000000000000000, 0.000000000000000000, 0.000000000000000000 ) ) ;
#6410 = EDGE_CURVE ( 'NONE', #4126, #11823, #5354, .T. ) ;
#6411 = CARTESIAN_POINT ( 'NONE',  ( 32.07500000054622546, 15.71886984736413417, 96.68563167572563088 ) ) ;
#6412 = CARTESIAN_POINT ( 'NONE',  ( 47.27500000054622831, 27.65831843345427998, 90.79316153445363113 ) ) ;
#6413 = CARTESIAN_POINT ( 'NONE',  ( 32.57500000054621836, 13.80429023900056684, 86.29171490190961435 ) ) ;
#6414 = CARTESIAN_POINT ( 'NONE',  ( 38.39999999999999147, 12.86707612778636012, 93.11078899226572503 ) ) ;
#6415 = CARTESIAN_POINT ( 'NONE',  ( 5.303296350723960551, 28.48414319546200346, 24.43259468344301055 ) ) ;
#6416 = CARTESIAN_POINT ( 'NONE',  ( 38.27500000054623541, 12.34168156654572535, 90.79316153445363113 ) ) ;
#6417 = VERTEX_POINT ( 'NONE', #11411 ) ;
#6418 = CARTESIAN_POINT ( 'NONE',  ( 19.95000000109246230, 13.62011893735971135, 95.42841645007781892 ) ) ;
#6419 = DIRECTION ( 'NONE',  ( 0.000000000000000000, 0.000000000000000000, -1.000000000000000000 ) ) ;
#6420 = ORIENTED_EDGE ( 'NONE', *, *, #11765, .F. ) ;
#6421 = EDGE_CURVE ( 'NONE', #3740, #8586, #3834, .T. ) ;
#6422 = FACE_OUTER_BOUND ( 'NONE', #623, .T. ) ;
#6423 = EDGE_LOOP ( 'NONE', ( #8068, #6775, #12029, #6305, #1921 ) ) ;
#6424 = CARTESIAN_POINT ( 'NONE',  ( -50.00000000000001421, 69.50000000000000000, 146.8533255156881978 ) ) ;
#6425 = CARTESIAN_POINT ( 'NONE',  ( 20.95000000109246230, 26.37988106264029398, 86.15790661882942914 ) ) ;
#6426 = EDGE_CURVE ( 'NONE', #5428, #1420, #6523, .T. ) ;
#6427 = CARTESIAN_POINT ( 'NONE',  ( 4.330144968755956114, 47.49467013450670549, -27.66326046019273832 ) ) ;
#6428 = CARTESIAN_POINT ( 'NONE',  ( 6.000000000000000000, 0.000000000000000000, 0.000000000000000000 ) ) ;
#6429 = AXIS2_PLACEMENT_3D ( 'NONE', #5931, #5870, #5108 ) ;
#6430 = CARTESIAN_POINT ( 'NONE',  ( 27.07500000054622902, 26.19570976099943493, 86.29171490190961435 ) ) ;
#6431 = CARTESIAN_POINT ( 'NONE',  ( 25.37500000054622618, 27.65831843345427998, 90.79316153445363113 ) ) ;
#6432 = CARTESIAN_POINT ( 'NONE',  ( -3.294598684565033704E-22, 45.00000000000000711, -28.00000000000000355 ) ) ;
#6433 = ORIENTED_EDGE ( 'NONE', *, *, #11782, .F. ) ;
#6434 = CARTESIAN_POINT ( 'NONE',  ( 37.75000000109246656, 17.56310227825320425, 98.29316153445363113 ) ) ;
#6435 = FILL_AREA_STYLE ('',( #3761 ) ) ;
#6436 = VERTEX_POINT ( 'NONE', #12366 ) ;
#6437 = CARTESIAN_POINT ( 'NONE',  ( 7.192769615190809278E-19, 10.00000000000000000, -28.00000000000000355 ) ) ;
#6438 = ORIENTED_EDGE ( 'NONE', *, *, #160, .T. ) ;
#6439 = AXIS2_PLACEMENT_3D ( 'NONE', #7693, #2167, #2098 ) ;
#6440 = CARTESIAN_POINT ( 'NONE',  ( 5.000000000000000000, 4.685197434473814759, -5.637851296924623057E-15 ) ) ;
#6441 = CARTESIAN_POINT ( 'NONE',  ( 0.3289161358670515400, 10.00000000000000355, -25.00000000000000711 ) ) ;
#6442 = CARTESIAN_POINT ( 'NONE',  ( 29.09999999999998721, 22.43689772174679575, 83.29316153445363113 ) ) ;
#6443 = AXIS2_PLACEMENT_3D ( 'NONE', #979, #7886, #10793 ) ;
#6444 = EDGE_CURVE ( 'NONE', #11432, #6932, #8616, .T. ) ;
#6445 = CARTESIAN_POINT ( 'NONE',  ( 38.65000000109246514, 20.00000000000000355, 83.29316153445364534 ) ) ;
#6446 = LINE ( 'NONE', #1868, #4430 ) ;
#6447 = CARTESIAN_POINT ( 'NONE',  ( -9.655964325742520060, 17.37895558718825129, 18.64870055153495798 ) ) ;
#6448 = DIRECTION ( 'NONE',  ( 0.000000000000000000, 1.000000000000000000, 0.000000000000000000 ) ) ;
#6449 = CARTESIAN_POINT ( 'NONE',  ( 25.57500000054622546, 24.28113015263587116, 96.68563167572563088 ) ) ;
#6450 = CARTESIAN_POINT ( 'NONE',  ( 6.112888882359681197, 27.94072674827362590, 24.24745615746033423 ) ) ;
#6451 = EDGE_CURVE ( 'NONE', #3740, #8002, #2659, .T. ) ;
#6452 = FACE_OUTER_BOUND ( 'NONE', #4164, .T. ) ;
#6453 = VERTEX_POINT ( 'NONE', #11598 ) ;
#6454 = ADVANCED_FACE ( 'NONE', ( #10390 ), #2220, .T. ) ;
#6455 = CIRCLE ( 'NONE', #384, 21.00000000000000000 ) ;
#6456 = LINE ( 'NONE', #560, #7636 ) ;
#6457 = CARTESIAN_POINT ( 'NONE',  ( 6.000000000000000000, 4.379923479639795225, -2.528750000000006271 ) ) ;
#6458 = CARTESIAN_POINT ( 'NONE',  ( 38.57500000054622546, 15.71886984736413773, 84.90069139318163138 ) ) ;
#6459 = CARTESIAN_POINT ( 'NONE',  ( 35.67500000054622689, 24.28113015263587116, 96.68563167572563088 ) ) ;
#6460 = CARTESIAN_POINT ( 'NONE',  ( 29.67500000054623044, 22.36655054427230027, 98.07665518445361386 ) ) ;
#6461 = AXIS2_PLACEMENT_3D ( 'NONE', #199, #7162, #4055 ) ;
#6462 = CARTESIAN_POINT ( 'NONE',  ( -50.00000000000001421, 40.00000000000000000, 169.9999999999999716 ) ) ;
#6463 = CARTESIAN_POINT ( 'NONE',  ( -10.00000000000000355, 20.00000000000000355, 22.91287847477919826 ) ) ;
#6464 = CARTESIAN_POINT ( 'NONE',  ( 33.59999999999999432, 27.13292387221364876, 93.11078899226573924 ) ) ;
#6465 = FACE_OUTER_BOUND ( 'NONE', #12460, .T. ) ;
#6466 = VERTEX_POINT ( 'NONE', #2779 ) ;
#6467 = CARTESIAN_POINT ( 'NONE',  ( 12.00000000000000000, 8.082668874372534964E-16, 6.600000000000003197 ) ) ;
#6468 = ORIENTED_EDGE ( 'NONE', *, *, #4679, .F. ) ;
#6469 = CARTESIAN_POINT ( 'NONE',  ( 10.40000000000000036, 0.000000000000000000, -5.400000000000001243 ) ) ;
#6470 = APPLICATION_PROTOCOL_DEFINITION ( 'draft international standard', 'automotive_design', 1998, #9350 ) ;
#6471 = CARTESIAN_POINT ( 'NONE',  ( 29.77500000054621765, 22.36655054427230027, 98.07665518445361386 ) ) ;
#6472 = DIRECTION ( 'NONE',  ( 1.000000000000000000, -0.000000000000000000, -0.000000000000000000 ) ) ;
#6473 = CARTESIAN_POINT ( 'NONE',  ( 43.87500000054622973, 17.63344945572769973, 98.07665518445361386 ) ) ;
#6474 = CARTESIAN_POINT ( 'NONE',  ( 31.97500000054622760, 17.63344945572769973, 98.07665518445361386 ) ) ;
#6475 = CARTESIAN_POINT ( 'NONE',  ( 30.99999999999998934, 20.00000000000000355, 83.29316153445364534 ) ) ;
#6476 = CARTESIAN_POINT ( 'NONE',  ( -4.158531974891625183, 29.10015071429011613, 20.58640575284740493 ) ) ;
#6477 = CARTESIAN_POINT ( 'NONE',  ( 38.67500000054623399, 17.63344945572770328, 83.50966788445364841 ) ) ;
#6478 = ORIENTED_EDGE ( 'NONE', *, *, #12427, .T. ) ;
#6479 = CARTESIAN_POINT ( 'NONE',  ( 48.97500000054622404, 24.28113015263587471, 84.90069139318163138 ) ) ;
#6480 = FACE_OUTER_BOUND ( 'NONE', #5884, .T. ) ;
#6481 = ORIENTED_EDGE ( 'NONE', *, *, #4823, .F. ) ;
#6482 = CYLINDRICAL_SURFACE ( 'NONE', #11772, 5.000000000000000888 ) ;
#6483 = ORIENTED_EDGE ( 'NONE', *, *, #7695, .F. ) ;
#6484 = CARTESIAN_POINT ( 'NONE',  ( 8.654532730718658584, 25.02058024782134282, -23.45477484801500623 ) ) ;
#6485 = CARTESIAN_POINT ( 'NONE',  ( 27.49999999999999645, 20.00000000000000355, 170.0000000000000000 ) ) ;
#6486 = CARTESIAN_POINT ( 'NONE',  ( 10.00000000000000355, 20.00000000000000355, -26.15339366124404208 ) ) ;
#6487 = PRESENTATION_LAYER_ASSIGNMENT (  '', '', ( #1626 ) ) ;
#6488 = FACE_OUTER_BOUND ( 'NONE', #8408, .T. ) ;
#6489 = EDGE_CURVE ( 'NONE', #10467, #10935, #9700, .T. ) ;
#6490 = CARTESIAN_POINT ( 'NONE',  ( 24.67500000054622689, 17.63344945572770328, 83.50966788445364841 ) ) ;
#6491 = CARTESIAN_POINT ( 'NONE',  ( 48.89999999999999147, 17.56310227825321135, 83.29316153445363113 ) ) ;
#6492 = DIRECTION ( 'NONE',  ( -0.000000000000000000, 1.336710962791342904E-15, 1.000000000000000000 ) ) ;
#6493 = CARTESIAN_POINT ( 'NONE',  ( 0.000000000000000000, 20.00000000000000355, -28.00000000000000711 ) ) ;
#6494 = ORIENTED_EDGE ( 'NONE', *, *, #6380, .F. ) ;
#6495 = CARTESIAN_POINT ( 'NONE',  ( 36.95000000109246230, 26.37988106264029398, 86.15790661882942914 ) ) ;
#6496 = DIRECTION ( 'NONE',  ( 1.000000000000000000, -0.000000000000000000, 0.000000000000000000 ) ) ;
#6497 = ORIENTED_EDGE ( 'NONE', *, *, #8153, .F. ) ;
#6498 = DIRECTION ( 'NONE',  ( 0.000000000000000000, 0.000000000000000000, -1.000000000000000000 ) ) ;
#6499 = ORIENTED_EDGE ( 'NONE', *, *, #3662, .T. ) ;
#6500 = CARTESIAN_POINT ( 'NONE',  ( -1.314141907159803946, 10.08123752450589095, -24.96759818712484957 ) ) ;
#6501 = CARTESIAN_POINT ( 'NONE',  ( 9.983665930786834508, 19.33914921762187689, -18.47505920260298851 ) ) ;
#6502 = CARTESIAN_POINT ( 'NONE',  ( 53.99999999999999289, 20.00000000000000355, 170.9999999999999716 ) ) ;
#6503 = AXIS2_PLACEMENT_3D ( 'NONE', #10985, #12000, #11938 ) ;
#6504 = DIRECTION ( 'NONE',  ( 1.000000000000000000, 0.000000000000000000, 0.000000000000000000 ) ) ;
#6505 = DIRECTION ( 'NONE',  ( 0.000000000000000000, -1.000000000000000000, 1.039664082171044481E-15 ) ) ;
#6506 = EDGE_CURVE ( 'NONE', #6002, #1723, #4620, .T. ) ;
#6507 = DIRECTION ( 'NONE',  ( 0.000000000000000000, 0.000000000000000000, -1.000000000000000000 ) ) ;
#6508 = CARTESIAN_POINT ( 'NONE',  ( 6.000000000000000000, -2.919948986426523341, 5.057500000000002771 ) ) ;
#6509 = CARTESIAN_POINT ( 'NONE',  ( 47.57500000054621125, 26.19570976099943493, 95.29460816699764791 ) ) ;
#6510 = CARTESIAN_POINT ( 'NONE',  ( 8.124594680848492345, 25.83911103074633075, 23.64375881965231230 ) ) ;
#6511 = CARTESIAN_POINT ( 'NONE',  ( 0.000000000000000000, 0.000000000000000000, -21.00000000000000000 ) ) ;
#6512 = ORIENTED_EDGE ( 'NONE', *, *, #5253, .T. ) ;
#6513 = LINE ( 'NONE', #12051, #7020 ) ;
#6514 =( BOUNDED_CURVE ( )  B_SPLINE_CURVE ( 3, ( #5947, #8865, #1136, #9887 ),
 .UNSPECIFIED., .F., .F. ) 
 B_SPLINE_CURVE_WITH_KNOTS ( ( 4, 4 ),
 ( 3.411525449423196132, 4.712388980384689674 ),
 .UNSPECIFIED. ) 
 CURVE ( )  GEOMETRIC_REPRESENTATION_ITEM ( )  RATIONAL_B_SPLINE_CURVE ( ( 1.000000000000000000, 0.8638816171694809753, 0.8638816171694809753, 1.000000000000000000 ) ) 
 REPRESENTATION_ITEM ( '' )  );
#6515 = CARTESIAN_POINT ( 'NONE',  ( 5.000000000000000000, 50.00000000000000000, 24.49489742783178059 ) ) ;
#6516 = CARTESIAN_POINT ( 'NONE',  ( 34.37500000054622973, 13.07298590277314432, 88.54243821818161564 ) ) ;
#6517 = CARTESIAN_POINT ( 'NONE',  ( 40.17500000054622689, 13.80429023900056507, 95.29460816699764791 ) ) ;
#6518 = CARTESIAN_POINT ( 'NONE',  ( 10.00000000000000355, 20.00000000000000355, 98.29316153445363113 ) ) ;
#6519 = CARTESIAN_POINT ( 'NONE',  ( 35.65000000109246514, 20.00000000000000355, 98.29316153445363113 ) ) ;
#6520 = CARTESIAN_POINT ( 'NONE',  ( -9.868806730738530320, 21.64797418619996350, 22.96979908047426377 ) ) ;
#6521 = EDGE_CURVE ( 'NONE', #10832, #8002, #10614, .T. ) ;
#6522 = CARTESIAN_POINT ( 'NONE',  ( 33.09999999999998010, 22.43689772174679575, 83.29316153445363113 ) ) ;
#6523 = LINE ( 'NONE', #7733, #9921 ) ;
#6524 = DIRECTION ( 'NONE',  ( -1.000000000000000000, -0.000000000000000000, -0.000000000000000000 ) ) ;
#6525 = FACE_OUTER_BOUND ( 'NONE', #2393, .T. ) ;
#6526 = EDGE_CURVE ( 'NONE', #9164, #9118, #10512, .T. ) ;
#6527 = CARTESIAN_POINT ( 'NONE',  ( 24.77500000054622475, 17.63344945572770328, 83.50966788445364841 ) ) ;
#6528 = DIRECTION ( 'NONE',  ( 0.000000000000000000, -1.000000000000000000, 1.039664082171044875E-15 ) ) ;
#6529 = VECTOR ( 'NONE', #8310, 1000.000000000000000 ) ;
#6530 = CARTESIAN_POINT ( 'NONE',  ( 38.77500000054622831, 20.00000000000000355, 83.50966788445364841 ) ) ;
#6531 = ADVANCED_FACE ( 'NONE', ( #4686 ), #10637, .F. ) ;
#6532 = CARTESIAN_POINT ( 'NONE',  ( 26.17500000054622689, 13.80429023900056507, 95.29460816699764791 ) ) ;
#6533 = CARTESIAN_POINT ( 'NONE',  ( 31.19999999999998863, 24.40838939219355197, 84.72553407664153724 ) ) ;
#6534 = CARTESIAN_POINT ( 'NONE',  ( 7.931687869515056555, 26.09867752937626406, 23.70939416258605803 ) ) ;
#6535 = CARTESIAN_POINT ( 'NONE',  ( 42.57500000054623257, 15.71886984736413773, 84.90069139318163138 ) ) ;
#6536 = ORIENTED_EDGE ( 'NONE', *, *, #7004, .T. ) ;
#6537 = CARTESIAN_POINT ( 'NONE',  ( 47.27500000054622831, 27.65831843345427998, 90.79316153445363113 ) ) ;
#6538 = DIRECTION ( 'NONE',  ( 0.000000000000000000, 0.000000000000000000, 1.000000000000000000 ) ) ;
#6539 = EDGE_LOOP ( 'NONE', ( #5967, #8270, #253, #10169, #12196 ) ) ;
#6540 = CARTESIAN_POINT ( 'NONE',  ( 6.605462518297898100, 12.48519332047425578, 19.93580698149260400 ) ) ;
#6541 = ORIENTED_EDGE ( 'NONE', *, *, #9788, .F. ) ;
#6542 = CIRCLE ( 'NONE', #9594, 4.057500000000000107 ) ;
#6543 = DIRECTION ( 'NONE',  ( 0.000000000000000000, 0.000000000000000000, 1.000000000000000000 ) ) ;
#6544 = DIRECTION ( 'NONE',  ( -1.000000000000000000, -0.000000000000000000, -0.000000000000000000 ) ) ;
#6545 = CARTESIAN_POINT ( 'NONE',  ( 20.27158385259953377, 22.00000000000000000, 152.2284161474004520 ) ) ;
#6546 = EDGE_CURVE ( 'NONE', #5153, #4064, #5829, .T. ) ;
#6547 = CARTESIAN_POINT ( 'NONE',  ( 43.17500000054621978, 26.19570976099943849, 86.29171490190961435 ) ) ;
#6548 = CARTESIAN_POINT ( 'NONE',  ( 20.59999999999998721, 12.86707612778636012, 88.47553407664152303 ) ) ;
#6549 = CARTESIAN_POINT ( 'NONE',  ( 23.87500000054622973, 17.63344945572769973, 98.07665518445361386 ) ) ;
#6550 = CARTESIAN_POINT ( 'NONE',  ( 47.19999999999998863, 24.40838939219355197, 84.72553407664153724 ) ) ;
#6551 = AXIS2_PLACEMENT_3D ( 'NONE', #9813, #998, #3212 ) ;
#6552 = FACE_OUTER_BOUND ( 'NONE', #9303, .T. ) ;
#6553 = CARTESIAN_POINT ( 'NONE',  ( 6.000000000000000000, 0.000000000000000000, 0.000000000000000000 ) ) ;
#6554 = ORIENTED_EDGE ( 'NONE', *, *, #879, .F. ) ;
#6555 = CARTESIAN_POINT ( 'NONE',  ( 36.45000000109246940, 15.59161060780646046, 84.72553407664153724 ) ) ;
#6556 = CARTESIAN_POINT ( 'NONE',  ( 9.659257073854845999, 17.39080730681331488, 23.05883108104414347 ) ) ;
#6557 = VERTEX_POINT ( 'NONE', #4876 ) ;
#6558 = CARTESIAN_POINT ( 'NONE',  ( 49.99999999999998579, 0.000000000000000000, 69.99999999999998579 ) ) ;
#6559 = EDGE_LOOP ( 'NONE', ( #3130, #7501, #8055, #6586 ) ) ;
#6560 = EDGE_CURVE ( 'NONE', #2695, #10935, #1266, .T. ) ;
#6561 = CARTESIAN_POINT ( 'NONE',  ( -9.983516779091171855, 19.33659569722678029, -22.92009366892111899 ) ) ;
#6562 = AXIS2_PLACEMENT_3D ( 'NONE', #6243, #2374, #3322 ) ;
#6563 = FACE_OUTER_BOUND ( 'NONE', #10549, .T. ) ;
#6564 = CIRCLE ( 'NONE', #12045, 6.500000000000000888 ) ;
#6565 = CARTESIAN_POINT ( 'NONE',  ( -9.673352204464322313, 22.61971715202064104, 23.05311956053869338 ) ) ;
#6566 = DIRECTION ( 'NONE',  ( -1.000000000000000000, -0.000000000000000000, -0.000000000000000000 ) ) ;
#6567 = CARTESIAN_POINT ( 'NONE',  ( -5.000000000000004441, 40.00000000000000000, 169.9999999999999716 ) ) ;
#6568 = CARTESIAN_POINT ( 'NONE',  ( -2.000000000000015543, 20.00000000000000355, 98.29316153445363113 ) ) ;
#6569 = DIRECTION ( 'NONE',  ( 1.000000000000000000, 0.000000000000000000, 0.000000000000000000 ) ) ;
#6570 = CARTESIAN_POINT ( 'NONE',  ( 21.57500000054622546, 24.28113015263587116, 96.68563167572563088 ) ) ;
#6571 = CARTESIAN_POINT ( 'NONE',  ( 46.25000000109246656, 12.86707612778636012, 88.47553407664152303 ) ) ;
#6572 = AXIS2_PLACEMENT_3D ( 'NONE', #12203, #10117, #2551 ) ;
#6573 = DIRECTION ( 'NONE',  ( -0.000000000000000000, 0.8660254037844393737, 0.4999999999999987232 ) ) ;
#6574 = VERTEX_POINT ( 'NONE', #6016 ) ;
#6575 = VERTEX_POINT ( 'NONE', #3031 ) ;
#6576 = CARTESIAN_POINT ( 'NONE',  ( -9.351975853621407708, 23.55614770899448374, -18.80319155380984242 ) ) ;
#6577 = ADVANCED_FACE ( 'NONE', ( #7857 ), #11207, .T. ) ;
#6578 = DIRECTION ( 'NONE',  ( -0.000000000000000000, 0.000000000000000000, 1.000000000000000000 ) ) ;
#6579 = CARTESIAN_POINT ( 'NONE',  ( 37.67500000054621978, 24.28113015263587116, 96.68563167572563088 ) ) ;
#6580 = CARTESIAN_POINT ( 'NONE',  ( 20.47500000054622760, 13.80429023900056684, 86.29171490190961435 ) ) ;
#6581 = DIRECTION ( 'NONE',  ( 0.000000000000000000, 0.000000000000000000, 1.000000000000000000 ) ) ;
#6582 = CARTESIAN_POINT ( 'NONE',  ( 0.000000000000000000, -5.839897972853060892, 7.806255641895631925E-15 ) ) ;
#6583 = CARTESIAN_POINT ( 'NONE',  ( -0.6576844598599284053, 54.96731546091645271, -20.99214996227340180 ) ) ;
#6584 = DIRECTION ( 'NONE',  ( -0.7071067811865489050, -0.000000000000000000, -0.7071067811865460184 ) ) ;
#6585 = CARTESIAN_POINT ( 'NONE',  ( 34.65000000109246514, 20.00000000000000355, 83.29316153445364534 ) ) ;
#6586 = ORIENTED_EDGE ( 'NONE', *, *, #11552, .F. ) ;
#6587 = LINE ( 'NONE', #5647, #1455 ) ;
#6588 = DIRECTION ( 'NONE',  ( -0.000000000000000000, -0.000000000000000000, 1.000000000000000000 ) ) ;
#6589 = CARTESIAN_POINT ( 'NONE',  ( 37.77500000054623541, 20.00000000000000355, 98.07665518445361386 ) ) ;
#6590 = CARTESIAN_POINT ( 'NONE',  ( 28.67500000054622689, 15.71886984736413773, 84.90069139318163138 ) ) ;
#6591 = CARTESIAN_POINT ( 'NONE',  ( 29.09999999999998721, 22.43689772174679575, 83.29316153445363113 ) ) ;
#6592 = ADVANCED_FACE ( 'NONE', ( #4936 ), #8176, .T. ) ;
#6593 = CARTESIAN_POINT ( 'NONE',  ( 33.99999999999998579, 20.00000000000000355, 98.29316153445363113 ) ) ;
#6594 = CARTESIAN_POINT ( 'NONE',  ( 39.17500000054623399, 26.92701409722686634, 88.54243821818162985 ) ) ;
#6595 = ORIENTED_EDGE ( 'NONE', *, *, #1352, .F. ) ;
#6596 = CARTESIAN_POINT ( 'NONE',  ( 48.37500000054622973, 13.07298590277314432, 88.54243821818161564 ) ) ;
#6597 = CARTESIAN_POINT ( 'NONE',  ( -5.000000000000000888, 0.000000000000000000, 169.9999999999999716 ) ) ;
#6598 = ORIENTED_EDGE ( 'NONE', *, *, #1939, .T. ) ;
#6599 = CARTESIAN_POINT ( 'NONE',  ( -2.601079580437228422, 29.66139515859289233, -27.88071816736361441 ) ) ;
#6600 = ORIENTED_EDGE ( 'NONE', *, *, #11811, .F. ) ;
#6601 = EDGE_CURVE ( 'NONE', #9736, #3374, #2072, .T. ) ;
#6602 = CARTESIAN_POINT ( 'NONE',  ( 42.35000000109246798, 13.62011893735970958, 86.15790661882942914 ) ) ;
#6603 = DIRECTION ( 'NONE',  ( 0.000000000000000000, 0.000000000000000000, -1.000000000000000000 ) ) ;
#6604 = CARTESIAN_POINT ( 'NONE',  ( 2.509417286374489020, 45.66310105023414678, -27.88864816121832746 ) ) ;
#6605 = CARTESIAN_POINT ( 'NONE',  ( 43.07500000054622546, 24.28113015263587471, 84.90069139318163138 ) ) ;
#6606 = CARTESIAN_POINT ( 'NONE',  ( 20.29999999999998650, 13.62011893735970958, 95.42841645007781892 ) ) ;
#6607 = DIRECTION ( 'NONE',  ( 1.000000000000000000, 0.000000000000000000, 0.000000000000000000 ) ) ;
#6608 = CARTESIAN_POINT ( 'NONE',  ( 45.77500000054622120, 22.36655054427230027, 98.07665518445361386 ) ) ;
#6609 = CARTESIAN_POINT ( 'NONE',  ( 20.17500000054622689, 13.80429023900056507, 95.29460816699764791 ) ) ;
#6610 = CIRCLE ( 'NONE', #12096, 13.85889894354065355 ) ;
#6611 = CARTESIAN_POINT ( 'NONE',  ( -1.324565580760808992, 29.93364609169914914, -24.97324923543901320 ) ) ;
#6612 = CARTESIAN_POINT ( 'NONE',  ( 19.99999999999998579, 20.00000000000000355, 98.29316153445363113 ) ) ;
#6613 = VERTEX_POINT ( 'NONE', #5070 ) ;
#6614 = CARTESIAN_POINT ( 'NONE',  ( 40.35000000109246798, 13.62011893735971135, 86.15790661882942914 ) ) ;
#6615 = CARTESIAN_POINT ( 'NONE',  ( 2.508429781980343609, 54.33777489521010295, -24.87536199211671573 ) ) ;
#6616 = ORIENTED_EDGE ( 'NONE', *, *, #6220, .F. ) ;
#6617 = DIRECTION ( 'NONE',  ( 0.000000000000000000, 0.000000000000000000, 1.000000000000000000 ) ) ;
#6618 = ORIENTED_EDGE ( 'NONE', *, *, #905, .F. ) ;
#6619 = CARTESIAN_POINT ( 'NONE',  ( -6.610481451048220158, 27.51047402958706201, -24.11159121895188306 ) ) ;
#6620 = VECTOR ( 'NONE', #11562, 1000.000000000000000 ) ;
#6621 = DIRECTION ( 'NONE',  ( 1.000000000000000000, 0.000000000000000000, 0.000000000000000000 ) ) ;
#6622 = CARTESIAN_POINT ( 'NONE',  ( 6.000000000000000000, -2.919948986426523341, 5.057500000000002771 ) ) ;
#6623 = CARTESIAN_POINT ( 'NONE',  ( 0.000000000000000000, 20.00000000000000355, 106.9999999999999574 ) ) ;
#6624 = CARTESIAN_POINT ( 'NONE',  ( -0.6600009463833134138, 45.03295123165366931, 20.99208596347618538 ) ) ;
#6625 = ORIENTED_EDGE ( 'NONE', *, *, #2085, .T. ) ;
#6626 = CARTESIAN_POINT ( 'NONE',  ( 5.000000000000000000, 50.00000000000000000, -27.54995462791182703 ) ) ;
#6627 = CYLINDRICAL_SURFACE ( 'NONE', #8989, 5.000000000000000000 ) ;
#6628 = CARTESIAN_POINT ( 'NONE',  ( 21.27500000054622831, 27.65831843345427998, 90.79316153445363113 ) ) ;
#6629 = VECTOR ( 'NONE', #691, 999.9999999999998863 ) ;
#6630 = DIRECTION ( 'NONE',  ( 0.000000000000000000, 0.000000000000000000, 1.000000000000000000 ) ) ;
#6631 = DIRECTION ( 'NONE',  ( 0.000000000000000000, 0.000000000000000000, -1.000000000000000000 ) ) ;
#6632 = ORIENTED_EDGE ( 'NONE', *, *, #2079, .T. ) ;
#6633 = VERTEX_POINT ( 'NONE', #8935 ) ;
#6634 = AXIS2_PLACEMENT_3D ( 'NONE', #4923, #8724, #6065 ) ;
#6635 = DIRECTION ( 'NONE',  ( 1.000000000000000000, -0.000000000000000000, -0.000000000000000000 ) ) ;
#6636 = CYLINDRICAL_SURFACE ( 'NONE', #10667, 5.999999999999999112 ) ;
#6637 = CARTESIAN_POINT ( 'NONE',  ( 5.000000000000000000, 0.000000000000000000, 0.000000000000000000 ) ) ;
#6638 = ADVANCED_FACE ( 'NONE', ( #3979 ), #8868, .F. ) ;
#6639 = CARTESIAN_POINT ( 'NONE',  ( 9.685273772782807100, 17.49881738785535745, 97.86827095828408574 ) ) ;
#6640 = DIRECTION ( 'NONE',  ( 0.000000000000000000, 0.000000000000000000, -1.000000000000000000 ) ) ;
#6641 = CARTESIAN_POINT ( 'NONE',  ( 5.000000000000000000, 4.685197434473814759, -5.637851296924623057E-15 ) ) ;
#6642 = CARTESIAN_POINT ( 'NONE',  ( 26.05000000109246727, 12.86707612778636012, 93.11078899226572503 ) ) ;
#6643 = AXIS2_PLACEMENT_3D ( 'NONE', #5766, #9635, #690 ) ;
#6644 = CARTESIAN_POINT ( 'NONE',  ( 0.6608155348566246978, 10.00000000000000178, 24.99999999999999645 ) ) ;
#6645 = ORIENTED_EDGE ( 'NONE', *, *, #12180, .T. ) ;
#6646 = CYLINDRICAL_SURFACE ( 'NONE', #3604, 5.000000000000000000 ) ;
#6647 = DIRECTION ( 'NONE',  ( 1.000000000000000000, 0.000000000000000000, 0.000000000000000000 ) ) ;
#6648 = AXIS2_PLACEMENT_3D ( 'NONE', #5923, #10601, #11632 ) ;
#6649 = CARTESIAN_POINT ( 'NONE',  ( 27.77500000054622475, 22.36655054427230027, 98.07665518445361386 ) ) ;
#6650 = CARTESIAN_POINT ( 'NONE',  ( 35.99999999999999289, 20.00000000000000355, 98.29316153445363113 ) ) ;
#6651 = CARTESIAN_POINT ( 'NONE',  ( 40.77500000054622831, 20.00000000000000355, 83.50966788445364841 ) ) ;
#6652 = AXIS2_PLACEMENT_3D ( 'NONE', #9491, #1620, #6321 ) ;
#6653 = CARTESIAN_POINT ( 'NONE',  ( 29.97500000054622404, 17.63344945572769973, 98.07665518445361386 ) ) ;
#6654 = CARTESIAN_POINT ( 'NONE',  ( 29.19999999999998508, 24.40838939219355197, 84.72553407664153724 ) ) ;
#6655 = CARTESIAN_POINT ( 'NONE',  ( 30.09999999999998721, 17.56310227825320425, 98.29316153445363113 ) ) ;
#6656 = CARTESIAN_POINT ( 'NONE',  ( 32.67500000054622689, 17.63344945572770328, 83.50966788445364841 ) ) ;
#6657 = EDGE_CURVE ( 'NONE', #3847, #2033, #1325, .T. ) ;
#6658 = EDGE_CURVE ( 'NONE', #801, #2755, #11853, .T. ) ;
#6659 = CARTESIAN_POINT ( 'NONE',  ( 46.47500000054623115, 13.80429023900056684, 86.29171490190961435 ) ) ;
#6660 = CARTESIAN_POINT ( 'NONE',  ( 28.35000000109246443, 13.62011893735970958, 86.15790661882942914 ) ) ;
#6661 = ORIENTED_EDGE ( 'NONE', *, *, #7930, .T. ) ;
#6662 = VECTOR ( 'NONE', #7070, 1000.000000000000000 ) ;
#6663 = CARTESIAN_POINT ( 'NONE',  ( 9.462075664854227242, 16.74749304780872450, 18.74782784431838323 ) ) ;
#6664 = ORIENTED_EDGE ( 'NONE', *, *, #9294, .T. ) ;
#6665 = CIRCLE ( 'NONE', #10315, 6.600000000000003197 ) ;
#6666 = CARTESIAN_POINT ( 'NONE',  ( -10.00000000000000355, 20.00000000000000355, -70.00000000000000000 ) ) ;
#6667 = CARTESIAN_POINT ( 'NONE',  ( 43.89999999999999147, 22.43689772174677088, 98.29316153445365956 ) ) ;
#6668 = EDGE_CURVE ( 'NONE', #2364, #6118, #10945, .T. ) ;
#6669 = CARTESIAN_POINT ( 'NONE',  ( 45.77500000054622120, 22.36655054427230027, 98.07665518445361386 ) ) ;
#6670 = CARTESIAN_POINT ( 'NONE',  ( -50.00000000000001421, 20.00000000000000000, 145.0000000000000000 ) ) ;
#6671 = LINE ( 'NONE', #12515, #5819 ) ;
#6672 = CARTESIAN_POINT ( 'NONE',  ( 42.67500000054622689, 15.71886984736413773, 84.90069139318163138 ) ) ;
#6673 = CARTESIAN_POINT ( 'NONE',  ( 47.69999999999999574, 26.37988106264029398, 95.42841645007781892 ) ) ;
#6674 = CARTESIAN_POINT ( 'NONE',  ( 12.59999999999999964, 0.000000000000000000, 0.000000000000000000 ) ) ;
#6675 = EDGE_CURVE ( 'NONE', #2798, #2989, #7794, .T. ) ;
#6676 = CARTESIAN_POINT ( 'NONE',  ( 0.000000000000000000, 0.000000000000000000, -25.00000000000000000 ) ) ;
#6677 = ORIENTED_EDGE ( 'NONE', *, *, #4049, .T. ) ;
#6678 = CARTESIAN_POINT ( 'NONE',  ( 39.45000000109246230, 24.40838939219354842, 96.86078899226572503 ) ) ;
#6679 = CARTESIAN_POINT ( 'NONE',  ( 1.620000493755592075, 54.74147302055352071, -24.94927790585931504 ) ) ;
#6680 = VERTEX_POINT ( 'NONE', #10699 ) ;
#6681 = CARTESIAN_POINT ( 'NONE',  ( 27.49999999999999645, 20.00000000000000355, 171.0000000000000000 ) ) ;
#6682 = ORIENTED_EDGE ( 'NONE', *, *, #2231, .F. ) ;
#6683 = CONICAL_SURFACE ( 'NONE', #7496, 5.057500000000000107, 1.047197551196592302 ) ;
#6684 = CARTESIAN_POINT ( 'NONE',  ( -50.00000000000001421, 55.00000000000000000, 166.8533255156881694 ) ) ;
#6685 = EDGE_CURVE ( 'NONE', #5212, #9148, #7920, .T. ) ;
#6686 = DIRECTION ( 'NONE',  ( -0.000000000000000000, -1.000000000000000000, -0.000000000000000000 ) ) ;
#6687 = CARTESIAN_POINT ( 'NONE',  ( -7.300087775502666965, 26.84214942138161675, 23.91163959704068631 ) ) ;
#6688 = EDGE_CURVE ( 'NONE', #2848, #5434, #1451, .T. ) ;
#6689 = DIRECTION ( 'NONE',  ( 1.000000000000000000, 0.000000000000000000, 0.000000000000000000 ) ) ;
#6690 = CARTESIAN_POINT ( 'NONE',  ( -4.967254743859118804, 49.34118944982712662, 20.40418484253504516 ) ) ;
#6691 = ORIENTED_EDGE ( 'NONE', *, *, #10824, .F. ) ;
#6692 = VECTOR ( 'NONE', #4817, 1000.000000000000114 ) ;
#6693 = CARTESIAN_POINT ( 'NONE',  ( 2.220191578079284245, 54.49201116149205149, -27.91348774472430705 ) ) ;
#6694 = CARTESIAN_POINT ( 'NONE',  ( -5.021298913057436586, 11.34591840113689365, 27.54762567907054205 ) ) ;
#6695 = CARTESIAN_POINT ( 'NONE',  ( 22.07500000054622546, 13.80429023900056507, 95.29460816699764791 ) ) ;
#6696 = ORIENTED_EDGE ( 'NONE', *, *, #2925, .F. ) ;
#6697 = DIRECTION ( 'NONE',  ( 1.000000000000000000, -0.000000000000000000, -0.000000000000000000 ) ) ;
#6698 = DIRECTION ( 'NONE',  ( -0.000000000000000000, -0.000000000000000000, 1.000000000000000000 ) ) ;
#6699 = ORIENTED_EDGE ( 'NONE', *, *, #6227, .T. ) ;
#6700 = ORIENTED_EDGE ( 'NONE', *, *, #9679, .T. ) ;
#6701 = AXIS2_PLACEMENT_3D ( 'NONE', #12063, #3365, #7232 ) ;
#6702 = CARTESIAN_POINT ( 'NONE',  ( -8.127963825975040635, 25.83452922977894772, -19.36426980763129180 ) ) ;
#6703 = DIRECTION ( 'NONE',  ( 1.000000000000000000, 0.000000000000000000, 0.000000000000000000 ) ) ;
#6704 = CARTESIAN_POINT ( 'NONE',  ( 20.97500000054622760, 24.28113015263587471, 84.90069139318163138 ) ) ;
#6705 = LINE ( 'NONE', #4617, #7469 ) ;
#6706 = FACE_OUTER_BOUND ( 'NONE', #6873, .T. ) ;
#6707 = CARTESIAN_POINT ( 'NONE',  ( 0.6528672473846522939, 45.03176223275875856, -20.99236587649955865 ) ) ;
#6708 = CARTESIAN_POINT ( 'NONE',  ( 25.95000000109246230, 13.62011893735970958, 95.42841645007781892 ) ) ;
#6709 = CARTESIAN_POINT ( 'NONE',  ( 0.000000000000000000, -2.919948986426525117, 5.057500000000004547 ) ) ;
#6710 = VERTEX_POINT ( 'NONE', #2518 ) ;
#6711 = CARTESIAN_POINT ( 'NONE',  ( 90.00000000000000000, 5.109226446042757607E-16, -4.171999999999999709 ) ) ;
#6712 = ADVANCED_FACE ( 'NONE', ( #10310 ), #3471, .F. ) ;
#6713 = CONTEXT_DEPENDENT_SHAPE_REPRESENTATION ( #834, #5296 ) ;
#6714 = CARTESIAN_POINT ( 'NONE',  ( 27.17500000054621623, 26.19570976099943849, 86.29171490190961435 ) ) ;
#6715 = CARTESIAN_POINT ( 'NONE',  ( 47.97500000054623115, 17.63344945572769973, 98.07665518445361386 ) ) ;
#6716 = CARTESIAN_POINT ( 'NONE',  ( 40.37500000054622973, 13.07298590277314432, 88.54243821818161564 ) ) ;
#6717 = CARTESIAN_POINT ( 'NONE',  ( 25.47500000054622404, 26.92701409722686634, 93.04388485072563242 ) ) ;
#6718 = CARTESIAN_POINT ( 'NONE',  ( 29.89999999999998437, 22.43689772174679575, 98.29316153445363113 ) ) ;
#6719 = CARTESIAN_POINT ( 'NONE',  ( 34.89999999999997726, 17.56310227825320425, 83.29316153445363113 ) ) ;
#6720 = CARTESIAN_POINT ( 'NONE',  ( 30.77500000054622831, 20.00000000000000355, 83.50966788445364841 ) ) ;
#6721 = VERTEX_POINT ( 'NONE', #8298 ) ;
#6722 = LINE ( 'NONE', #7874, #1430 ) ;
#6723 = VERTEX_POINT ( 'NONE', #11981 ) ;
#6724 = CARTESIAN_POINT ( 'NONE',  ( -50.00000000000001421, 18.00000000000000355, 152.2284161474004520 ) ) ;
#6725 = VERTEX_POINT ( 'NONE', #3287 ) ;
#6726 =( BOUNDED_CURVE ( )  B_SPLINE_CURVE ( 2, ( #1614, #663, #2875, #8711, #6736, #8833, #5798, #23, #6867, #88, #1048 ),
 .UNSPECIFIED., .F., .F. ) 
 B_SPLINE_CURVE_WITH_KNOTS ( ( 3, 2, 2, 2, 2, 3 ),
 ( 0.1666666666666665741, 0.1733333333333332560, 0.1799999999999999101, 0.1866666666666665919, 0.1933333333333332460, 0.1999999999999999278 ),
 .UNSPECIFIED. ) 
 CURVE ( )  GEOMETRIC_REPRESENTATION_ITEM ( )  RATIONAL_B_SPLINE_CURVE ( ( 1.000000000000000666, 0.9510565162951529761, 1.000000000000000000, 0.9510565162951535312, 1.000000000000000000, 0.9510565162951535312, 1.000000000000000000, 0.9510565162951535312, 1.000000000000000000, 0.9510565162951540863, 0.9999999999999994449 ) ) 
 REPRESENTATION_ITEM ( '' )  );
#6727 = FACE_BOUND ( 'NONE', #11523, .T. ) ;
#6728 = CARTESIAN_POINT ( 'NONE',  ( 1.642686742655169674, 10.13030119466746015, -27.95366245041864417 ) ) ;
#6729 = CARTESIAN_POINT ( 'NONE',  ( 44.77500000054622831, 17.63344945572770328, 83.50966788445364841 ) ) ;
#6730 = CARTESIAN_POINT ( 'NONE',  ( 20.39999999999998792, 12.86707612778636012, 93.11078899226572503 ) ) ;
#6731 = EDGE_CURVE ( 'NONE', #2943, #9959, #1688, .T. ) ;
#6732 = FILL_AREA_STYLE ('',( #1851 ) ) ;
#6733 = CARTESIAN_POINT ( 'NONE',  ( 44.07500000054622546, 15.71886984736413417, 96.68563167572563088 ) ) ;
#6734 = CARTESIAN_POINT ( 'NONE',  ( 46.59999999999998721, 12.86707612778636012, 88.47553407664152303 ) ) ;
#6735 = CARTESIAN_POINT ( 'NONE',  ( 45.99999999999998579, 20.00000000000000355, 98.29316153445363113 ) ) ;
#6736 = CARTESIAN_POINT ( 'NONE',  ( 44.59999999999998721, 12.86707612778636012, 88.47553407664152303 ) ) ;
#6737 = VERTEX_POINT ( 'NONE', #3405 ) ;
#6738 =( REPRESENTATION_RELATIONSHIP ('NONE','NONE', #4262, #8235 ) REPRESENTATION_RELATIONSHIP_WITH_TRANSFORMATION ( #8622 )SHAPE_REPRESENTATION_RELATIONSHIP( ) );
#6739 = ADVANCED_FACE ( 'NONE', ( #11024 ), #11086, .F. ) ;
#6740 = AXIS2_PLACEMENT_3D ( 'NONE', #11625, #2240, #973 ) ;
#6741 = CARTESIAN_POINT ( 'NONE',  ( 32.95000000109246230, 26.37988106264029398, 86.15790661882942914 ) ) ;
#6742 = DIRECTION ( 'NONE',  ( 0.000000000000000000, -0.000000000000000000, -1.000000000000000000 ) ) ;
#6743 = ORIENTED_EDGE ( 'NONE', *, *, #8159, .F. ) ;
#6744 =( NAMED_UNIT ( * ) SI_UNIT ( $, .STERADIAN. ) SOLID_ANGLE_UNIT ( ) );
#6745 = EDGE_LOOP ( 'NONE', ( #9566, #11179, #2146 ) ) ;
#6746 = DIRECTION ( 'NONE',  ( 1.000000000000000000, 0.000000000000000000, 0.000000000000000000 ) ) ;
#6747 = DIRECTION ( 'NONE',  ( 0.000000000000000000, 0.000000000000000000, -1.000000000000000000 ) ) ;
#6748 = DIRECTION ( 'NONE',  ( 0.000000000000000000, 1.000000000000000000, -1.039664082171044875E-15 ) ) ;
#6749 = VECTOR ( 'NONE', #5567, 1000.000000000000000 ) ;
#6750 = CARTESIAN_POINT ( 'NONE',  ( 37.47500000054623825, 26.19570976099943493, 95.29460816699764791 ) ) ;
#6751 = CARTESIAN_POINT ( 'NONE',  ( 5.028136979683376140, 28.66851506631811120, -27.55037744543317757 ) ) ;
#6752 = DIRECTION ( 'NONE',  ( 1.000000000000000000, 0.000000000000000000, 0.000000000000000000 ) ) ;
#6753 = ORIENTED_EDGE ( 'NONE', *, *, #4865, .F. ) ;
#6754 = DIRECTION ( 'NONE',  ( 0.000000000000000000, -1.000000000000000000, 0.000000000000000000 ) ) ;
#6755 = EDGE_CURVE ( 'NONE', #1521, #6176, #6542, .T. ) ;
#6756 = FACE_OUTER_BOUND ( 'NONE', #9863, .T. ) ;
#6757 = CARTESIAN_POINT ( 'NONE',  ( 47.97500000054623115, 17.63344945572769973, 98.07665518445361386 ) ) ;
#6758 = ORIENTED_EDGE ( 'NONE', *, *, #952, .T. ) ;
#6759 = CYLINDRICAL_SURFACE ( 'NONE', #7000, 7.500000000000000000 ) ;
#6760 = VECTOR ( 'NONE', #5607, 1000.000000000000000 ) ;
#6761 = EDGE_LOOP ( 'NONE', ( #8609, #12094, #3108, #6033 ) ) ;
#6762 = VECTOR ( 'NONE', #1404, 1000.000000000000000 ) ;
#6763 = VERTEX_POINT ( 'NONE', #8237 ) ;
#6764 = AXIS2_PLACEMENT_3D ( 'NONE', #7171, #10987, #10040 ) ;
#6765 = ADVANCED_FACE ( 'NONE', ( #7337 ), #7148, .F. ) ;
#6766 = CARTESIAN_POINT ( 'NONE',  ( 21.79999999999998650, 24.40838939219354842, 96.86078899226572503 ) ) ;
#6767 = DIRECTION ( 'NONE',  ( 0.000000000000000000, 0.4999999999999983902, -0.8660254037844395958 ) ) ;
#6768 = DIRECTION ( 'NONE',  ( -1.000000000000000000, -0.000000000000000000, -0.000000000000000000 ) ) ;
#6769 = CARTESIAN_POINT ( 'NONE',  ( 1.614286760591197245, 45.25655306502918762, -24.94965407877490549 ) ) ;
#6770 = CONICAL_SURFACE ( 'NONE', #1513, 28.00000000000000000, 0.7853981633974477239 ) ;
#6771 = CARTESIAN_POINT ( 'NONE',  ( -4.338943459110875089, 52.50631594060026686, -20.54770844439775956 ) ) ;
#6772 = CARTESIAN_POINT ( 'NONE',  ( -24.10660171779822747, 84.49999999999998579, 151.2467237978899846 ) ) ;
#6773 = CARTESIAN_POINT ( 'NONE',  ( 8.957954983704073726, 24.45660132507920537, -18.99431620520108766 ) ) ;
#6774 = CARTESIAN_POINT ( 'NONE',  ( 9.353363810095283171, 16.44731154698707698, 23.18475774758237407 ) ) ;
#6775 = ORIENTED_EDGE ( 'NONE', *, *, #2850, .T. ) ;
#6776 = CARTESIAN_POINT ( 'NONE',  ( 6.099398173400666145, 27.93114403207803420, -24.24592268179950594 ) ) ;
#6777 = UNCERTAINTY_MEASURE_WITH_UNIT (LENGTH_MEASURE( 1.000000000000000082E-05 ), #2294, 'distance_accuracy_value', 'NONE');
#6778 = CARTESIAN_POINT ( 'NONE',  ( 28.07500000054622546, 15.71886984736413417, 96.68563167572563088 ) ) ;
#6779 = DIRECTION ( 'NONE',  ( -0.000000000000000000, 1.000000000000000000, 1.224646799147353207E-16 ) ) ;
#6780 = CARTESIAN_POINT ( 'NONE',  ( 37.97500000054623115, 15.71886984736413417, 96.68563167572563088 ) ) ;
#6781 = CARTESIAN_POINT ( 'NONE',  ( 29.87500000054622618, 20.00000000000000355, 98.07665518445361386 ) ) ;
#6782 = CARTESIAN_POINT ( 'NONE',  ( 20.19999999999998863, 15.59161060780645691, 96.86078899226572503 ) ) ;
#6783 = EDGE_CURVE ( 'NONE', #2709, #2566, #6266, .T. ) ;
#6784 = CARTESIAN_POINT ( 'NONE',  ( 32.77500000054622831, 20.00000000000000355, 83.50966788445364841 ) ) ;
#6785 = ORIENTED_EDGE ( 'NONE', *, *, #1070, .F. ) ;
#6786 = PRODUCT ( 'MAS-314', 'MAS-314', '', ( #698 ) ) ;
#6787 = CIRCLE ( 'NONE', #2737, 8.000000000000000000 ) ;
#6788 = CARTESIAN_POINT ( 'NONE',  ( 5.000000000000000000, 0.000000000000000000, 0.000000000000000000 ) ) ;
#6789 = EDGE_LOOP ( 'NONE', ( #4326, #7309, #4351, #5025 ) ) ;
#6790 = VECTOR ( 'NONE', #6884, 1000.000000000000000 ) ;
#6791 = DIRECTION ( 'NONE',  ( -1.000000000000000000, -0.000000000000000000, -0.000000000000000000 ) ) ;
#6792 = ORIENTED_EDGE ( 'NONE', *, *, #8850, .T. ) ;
#6793 = DIRECTION ( 'NONE',  ( 0.000000000000000000, 0.000000000000000000, -1.000000000000000000 ) ) ;
#6794 = VECTOR ( 'NONE', #6985, 1000.000000000000000 ) ;
#6795 = CARTESIAN_POINT ( 'NONE',  ( 7.192769615190809278E-19, 10.00000000000000000, -28.00000000000000355 ) ) ;
#6796 = CARTESIAN_POINT ( 'NONE',  ( 45.57500000054621125, 26.19570976099943849, 95.29460816699764791 ) ) ;
#6797 = FACE_OUTER_BOUND ( 'NONE', #7166, .T. ) ;
#6798 = LINE ( 'NONE', #4905, #6620 ) ;
#6799 = CARTESIAN_POINT ( 'NONE',  ( 45.17500000054621978, 26.19570976099943493, 86.29171490190961435 ) ) ;
#6800 = CARTESIAN_POINT ( 'NONE',  ( 42.49999999999999289, 12.11403331821300533, 90.79316153445363113 ) ) ;
#6801 = CARTESIAN_POINT ( 'NONE',  ( 40.69999999999998863, 13.62011893735970958, 86.15790661882942914 ) ) ;
#6802 = EDGE_CURVE ( 'NONE', #12457, #7564, #8111, .T. ) ;
#6803 = DIRECTION ( 'NONE',  ( 0.000000000000000000, 0.5000000000000014433, 0.8660254037844379305 ) ) ;
#6804 = ORIENTED_EDGE ( 'NONE', *, *, #9909, .F. ) ;
#6805 = CARTESIAN_POINT ( 'NONE',  ( 32.45000000109246940, 15.59161060780646046, 84.72553407664153724 ) ) ;
#6806 = CARTESIAN_POINT ( 'NONE',  ( 6.955575927950914131E-22, 45.00000000000000711, -25.00000000000000000 ) ) ;
#6807 = ORIENTED_EDGE ( 'NONE', *, *, #4196, .F. ) ;
#6808 =( BOUNDED_CURVE ( )  B_SPLINE_CURVE ( 2, ( #4250, #11097, #8186, #5268, #5208, #4432, #5331, #5395, #2348, #7097, #9267 ),
 .UNSPECIFIED., .F., .F. ) 
 B_SPLINE_CURVE_WITH_KNOTS ( ( 3, 2, 2, 2, 2, 3 ),
 ( 0.1333333333333332205, 0.1399999999999999023, 0.1466666666666665564, 0.1533333333333332382, 0.1599999999999999201, 0.1666666666666665741 ),
 .UNSPECIFIED. ) 
 CURVE ( )  GEOMETRIC_REPRESENTATION_ITEM ( )  RATIONAL_B_SPLINE_CURVE ( ( 1.000000000000000888, 0.9510565162951527540, 1.000000000000000000, 0.9510565162951535312, 1.000000000000000000, 0.9510565162951535312, 1.000000000000000000, 0.9510565162951535312, 1.000000000000000000, 0.9510565162951541973, 0.9999999999999993339 ) ) 
 REPRESENTATION_ITEM ( '' )  );
#6809 = EDGE_CURVE ( 'NONE', #1877, #11818, #279, .T. ) ;
#6810 = VERTEX_POINT ( 'NONE', #3344 ) ;
#6811 = CARTESIAN_POINT ( 'NONE',  ( -3.709758735690515970E-18, 30.00000000000001066, -25.00000000000000000 ) ) ;
#6812 = CARTESIAN_POINT ( 'NONE',  ( -2.220795175011430533, 54.49171124227147089, -24.90301599942658228 ) ) ;
#6813 = DIRECTION ( 'NONE',  ( -0.5000000000000046629, 1.060575238724903587E-16, -0.8660254037844359321 ) ) ;
#6814 = CIRCLE ( 'NONE', #8246, 7.499999999999992895 ) ;
#6815 = EDGE_CURVE ( 'NONE', #169, #5431, #12023, .T. ) ;
#6816 = CARTESIAN_POINT ( 'NONE',  ( 37.57500000054622546, 24.28113015263587116, 96.68563167572563088 ) ) ;
#6817 = CARTESIAN_POINT ( 'NONE',  ( 38.27500000054622831, 13.07298590277314254, 93.04388485072563242 ) ) ;
#6818 = CARTESIAN_POINT ( 'NONE',  ( 44.15000000109246514, 12.11403331821300533, 90.79316153445363113 ) ) ;
#6819 = CARTESIAN_POINT ( 'NONE',  ( 4.999999999999997335, 20.00000000000000000, 145.0000000000000000 ) ) ;
#6820 = EDGE_LOOP ( 'NONE', ( #12489, #1277, #8350, #9794 ) ) ;
#6821 = EDGE_CURVE ( 'NONE', #12014, #1979, #5143, .T. ) ;
#6822 = CARTESIAN_POINT ( 'NONE',  ( 48.85000000109246088, 24.40838939219355197, 84.72553407664153724 ) ) ;
#6823 = PLANE ( 'NONE',  #5589 ) ;
#6824 = ORIENTED_EDGE ( 'NONE', *, *, #2977, .F. ) ;
#6825 = FACE_OUTER_BOUND ( 'NONE', #934, .T. ) ;
#6826 = EDGE_CURVE ( 'NONE', #9118, #4818, #4727, .T. ) ;
#6827 = EDGE_CURVE ( 'NONE', #10270, #6633, #8825, .T. ) ;
#6828 = VERTEX_POINT ( 'NONE', #5626 ) ;
#6829 = AXIS2_PLACEMENT_3D ( 'NONE', #2007, #5888, #1199 ) ;
#6830 = ORIENTED_EDGE ( 'NONE', *, *, #9294, .F. ) ;
#6831 = CARTESIAN_POINT ( 'NONE',  ( -9.463424455697749593, 23.24851154398614739, -18.74714503555872724 ) ) ;
#6832 = ADVANCED_FACE ( 'NONE', ( #5696 ), #12289, .F. ) ;
#6833 = DIRECTION ( 'NONE',  ( -0.000000000000000000, -0.000000000000000000, 1.000000000000000000 ) ) ;
#6834 = AXIS2_PLACEMENT_3D ( 'NONE', #7005, #162, #4019 ) ;
#6835 = CARTESIAN_POINT ( 'NONE',  ( 9.238455078247341135, 23.85215916112258228, 84.34042123683411774 ) ) ;
#6836 = LINE ( 'NONE', #9952, #11513 ) ;
#6837 = CARTESIAN_POINT ( 'NONE',  ( 27.49999999999999645, 20.00000000000000355, 188.9999999999999716 ) ) ;
#6838 = DIRECTION ( 'NONE',  ( -0.000000000000000000, -1.000000000000000000, -0.000000000000000000 ) ) ;
#6839 = EDGE_CURVE ( 'NONE', #589, #9944, #1151, .T. ) ;
#6840 = CARTESIAN_POINT ( 'NONE',  ( 26.25000000109246656, 12.86707612778636012, 88.47553407664152303 ) ) ;
#6841 = CARTESIAN_POINT ( 'NONE',  ( 5.000000000000000000, 0.000000000000000000, 4.057500000000000107 ) ) ;
#6842 = EDGE_LOOP ( 'NONE', ( #1587, #2470, #4366 ) ) ;
#6843 = CARTESIAN_POINT ( 'NONE',  ( 37.35000000109246088, 26.37988106264029398, 95.42841645007781892 ) ) ;
#6844 = CONTEXT_DEPENDENT_SHAPE_REPRESENTATION ( #2613, #10739 ) ;
#6845 = CARTESIAN_POINT ( 'NONE',  ( 19.97500000054622404, 17.63344945572769973, 98.07665518445361386 ) ) ;
#6846 = CARTESIAN_POINT ( 'NONE',  ( 49.67500000054622689, 24.28113015263587116, 96.68563167572563088 ) ) ;
#6847 = CARTESIAN_POINT ( 'NONE',  ( 34.47500000054623115, 13.80429023900056684, 86.29171490190961435 ) ) ;
#6848 = CIRCLE ( 'NONE', #3411, 13.85889894354065355 ) ;
#6849 = CARTESIAN_POINT ( 'NONE',  ( 24.17500000054622689, 13.80429023900056507, 95.29460816699764791 ) ) ;
#6850 = CARTESIAN_POINT ( 'NONE',  ( 25.29999999999998650, 26.37988106264029398, 86.15790661882942914 ) ) ;
#6851 = LINE ( 'NONE', #10524, #10707 ) ;
#6852 = CARTESIAN_POINT ( 'NONE',  ( 30.27500000054623186, 12.34168156654572535, 90.79316153445363113 ) ) ;
#6853 = ORIENTED_EDGE ( 'NONE', *, *, #5914, .F. ) ;
#6854 = FACE_OUTER_BOUND ( 'NONE', #786, .T. ) ;
#6855 = EDGE_LOOP ( 'NONE', ( #1750, #10407, #8775, #9220 ) ) ;
#6856 = DIRECTION ( 'NONE',  ( 1.000000000000000000, -0.000000000000000000, -0.000000000000000000 ) ) ;
#6857 = ORIENTED_EDGE ( 'NONE', *, *, #10906, .T. ) ;
#6858 = CIRCLE ( 'NONE', #10113, 5.400000000000001243 ) ;
#6859 = LINE ( 'NONE', #8958, #3749 ) ;
#6860 = CARTESIAN_POINT ( 'NONE',  ( 1.312601162367561303, 10.08103881020897319, -27.97114353547140908 ) ) ;
#6861 = CARTESIAN_POINT ( 'NONE',  ( 38.07500000054622546, 15.71886984736413417, 96.68563167572563088 ) ) ;
#6862 = FACE_OUTER_BOUND ( 'NONE', #114, .T. ) ;
#6863 = PLANE ( 'NONE',  #10262 ) ;
#6864 = CARTESIAN_POINT ( 'NONE',  ( 39.57500000054623257, 26.19570976099943493, 95.29460816699764791 ) ) ;
#6865 = CARTESIAN_POINT ( 'NONE',  ( 45.69999999999999574, 26.37988106264029398, 95.42841645007781892 ) ) ;
#6866 = CARTESIAN_POINT ( 'NONE',  ( 40.39999999999999147, 12.86707612778636012, 93.11078899226572503 ) ) ;
#6867 = CARTESIAN_POINT ( 'NONE',  ( 44.19999999999998863, 15.59161060780645691, 96.86078899226572503 ) ) ;
#6868 = PRESENTATION_LAYER_ASSIGNMENT (  '', '', ( #1005 ) ) ;
#6869 = ORIENTED_EDGE ( 'NONE', *, *, #11969, .T. ) ;
#6870 = CARTESIAN_POINT ( 'NONE',  ( 30.75000000109246301, 22.43689772174679575, 83.29316153445363113 ) ) ;
#6871 = CARTESIAN_POINT ( 'NONE',  ( 0.6608155348566246978, 10.00000000000000178, 24.99999999999999645 ) ) ;
#6872 = ORIENTED_EDGE ( 'NONE', *, *, #7376, .F. ) ;
#6873 = EDGE_LOOP ( 'NONE', ( #10683, #5539, #8510, #682, #11683 ) ) ;
#6874 = CARTESIAN_POINT ( 'NONE',  ( -9.740943735563897476, 22.28537929251632477, -23.02431258361445288 ) ) ;
#6875 = DIRECTION ( 'NONE',  ( 0.000000000000000000, 0.000000000000000000, 1.000000000000000000 ) ) ;
#6876 = EDGE_CURVE ( 'NONE', #1979, #7598, #932, .T. ) ;
#6877 = CARTESIAN_POINT ( 'NONE',  ( 6.000000000000000000, 6.193651186687738874E-16, -5.057500000000000107 ) ) ;
#6878 = CARTESIAN_POINT ( 'NONE',  ( 37.37500000054622973, 26.92701409722686634, 93.04388485072563242 ) ) ;
#6879 = CARTESIAN_POINT ( 'NONE',  ( 30.27500000054622475, 13.07298590277314254, 93.04388485072563242 ) ) ;
#6880 = CARTESIAN_POINT ( 'NONE',  ( 2.604960375799227901, 29.66039127547307785, -27.88036871804450101 ) ) ;
#6881 = CARTESIAN_POINT ( 'NONE',  ( 6.000000000000000000, 2.919948986426538884, 5.057499999999996554 ) ) ;
#6882 = ORIENTED_EDGE ( 'NONE', *, *, #1857, .F. ) ;
#6883 = CARTESIAN_POINT ( 'NONE',  ( 2.508429781980343609, 54.33777489521010295, -24.87536199211671573 ) ) ;
#6884 = DIRECTION ( 'NONE',  ( 1.000000000000000000, 0.000000000000000000, 0.000000000000000000 ) ) ;
#6885 = ORIENTED_EDGE ( 'NONE', *, *, #6657, .T. ) ;
#6886 = CARTESIAN_POINT ( 'NONE',  ( 5.000000000000000000, 3.513898075855356851, -2.028750000000006271 ) ) ;
#6887 = CIRCLE ( 'NONE', #809, 5.057500000000000107 ) ;
#6888 = ORIENTED_EDGE ( 'NONE', *, *, #6000, .F. ) ;
#6889 = ORIENTED_EDGE ( 'NONE', *, *, #9357, .F. ) ;
#6890 = DIRECTION ( 'NONE',  ( -0.000000000000000000, -0.000000000000000000, 1.000000000000000000 ) ) ;
#6891 = VECTOR ( 'NONE', #8315, 1000.000000000000000 ) ;
#6892 = CARTESIAN_POINT ( 'NONE',  ( -34.99999999999997868, 20.00000000000000000, 137.5000000000000000 ) ) ;
#6893 = EDGE_CURVE ( 'NONE', #7598, #8987, #6349, .T. ) ;
#6894 = CARTESIAN_POINT ( 'NONE',  ( 37.39999999999999147, 27.13292387221364876, 88.47553407664153724 ) ) ;
#6895 = CARTESIAN_POINT ( 'NONE',  ( 9.099320553259442335, 24.16039445067871583, 18.92675418898895501 ) ) ;
#6896 = CARTESIAN_POINT ( 'NONE',  ( 4.959250951056511703, 49.34212978433561858, -20.40603120131224557 ) ) ;
#6897 = LINE ( 'NONE', #7921, #11668 ) ;
#6898 = CARTESIAN_POINT ( 'NONE',  ( 41.27500000054622831, 27.65831843345427998, 90.79316153445363113 ) ) ;
#6899 = CARTESIAN_POINT ( 'NONE',  ( -6.999999999999999112, 77.00000000000000000, 94.35332551568819781 ) ) ;
#6900 = ORIENTED_EDGE ( 'NONE', *, *, #7131, .T. ) ;
#6901 = DIRECTION ( 'NONE',  ( 0.000000000000000000, 0.000000000000000000, 1.000000000000000000 ) ) ;
#6902 = SHAPE_DEFINITION_REPRESENTATION ( #2136, #4339 ) ;
#6903 = ADVANCED_FACE ( 'NONE', ( #803 ), #2893, .F. ) ;
#6904 = LINE ( 'NONE', #10770, #2558 ) ;
#6905 = DIRECTION ( 'NONE',  ( 0.000000000000000000, 0.000000000000000000, 1.000000000000000000 ) ) ;
#6906 = CARTESIAN_POINT ( 'NONE',  ( 33.27500000054622120, 27.65831843345427998, 90.79316153445363113 ) ) ;
#6907 = CARTESIAN_POINT ( 'NONE',  ( 5.307486386703490489, 11.51851869311760090, -24.43167369944409018 ) ) ;
#6908 = CARTESIAN_POINT ( 'NONE',  ( 25.49999999999998934, 27.88596668178699645, 90.79316153445363113 ) ) ;
#6909 = VECTOR ( 'NONE', #3548, 1000.000000000000000 ) ;
#6910 = CARTESIAN_POINT ( 'NONE',  ( 34.37500000054622973, 13.07298590277314432, 88.54243821818161564 ) ) ;
#6911 = VERTEX_POINT ( 'NONE', #3774 ) ;
#6912 = ADVANCED_FACE ( 'NONE', ( #6756 ), #6627, .F. ) ;
#6913 = FACE_OUTER_BOUND ( 'NONE', #5246, .T. ) ;
#6914 = ORIENTED_EDGE ( 'NONE', *, *, #2881, .T. ) ;
#6915 = CARTESIAN_POINT ( 'NONE',  ( 49.55000000109246372, 22.43689772174679575, 98.29316153445363113 ) ) ;
#6916 = ORIENTED_EDGE ( 'NONE', *, *, #3335, .F. ) ;
#6917 = DIRECTION ( 'NONE',  ( 0.000000000000000000, -0.000000000000000000, 1.000000000000000000 ) ) ;
#6918 = DIRECTION ( 'NONE',  ( 1.000000000000000000, 0.000000000000000000, 0.000000000000000000 ) ) ;
#6919 = EDGE_CURVE ( 'NONE', #4895, #11790, #2906, .T. ) ;
#6920 = CARTESIAN_POINT ( 'NONE',  ( 39.67500000054622689, 24.28113015263587116, 96.68563167572563088 ) ) ;
#6921 = CARTESIAN_POINT ( 'NONE',  ( 44.99999999999999289, 20.00000000000000355, 83.29316153445364534 ) ) ;
#6922 = LINE ( 'NONE', #6169, #10632 ) ;
#6923 =( BOUNDED_CURVE ( )  B_SPLINE_CURVE ( 2, ( #9028, #3120, #148, #7175, #11814, #10860, #4203, #10044, #7049, #2170, #10789 ),
 .UNSPECIFIED., .F., .F. ) 
 B_SPLINE_CURVE_WITH_KNOTS ( ( 3, 2, 2, 2, 2, 3 ),
 ( 0.7666666666666666075, 0.7733333333333332060, 0.7799999999999999156, 0.7866666666666666252, 0.7933333333333333348, 0.8000000000000000444 ),
 .UNSPECIFIED. ) 
 CURVE ( )  GEOMETRIC_REPRESENTATION_ITEM ( )  RATIONAL_B_SPLINE_CURVE ( ( 1.000000000000000888, 0.9510565162951527540, 1.000000000000000000, 0.9510565162951535312, 1.000000000000000000, 0.9510565162951535312, 1.000000000000000000, 0.9510565162951535312, 1.000000000000000000, 0.9510565162951535312, 1.000000000000000000 ) ) 
 REPRESENTATION_ITEM ( '' )  );
#6924 = CARTESIAN_POINT ( 'NONE',  ( 42.89999999999998437, 17.56310227825321135, 83.29316153445363113 ) ) ;
#6925 = CARTESIAN_POINT ( 'NONE',  ( -7.946065455725393356, 26.10639172058064972, -23.70672747870507280 ) ) ;
#6926 = DIRECTION ( 'NONE',  ( -0.000000000000000000, -0.000000000000000000, 1.000000000000000000 ) ) ;
#6927 = ORIENTED_EDGE ( 'NONE', *, *, #6783, .T. ) ;
#6928 = CARTESIAN_POINT ( 'NONE',  ( 34.35000000109246798, 13.62011893735971135, 86.15790661882942914 ) ) ;
#6929 = CARTESIAN_POINT ( 'NONE',  ( 3.548862490157215444, 10.64523530928737749, 24.74869899623665503 ) ) ;
#6930 = ORIENTED_EDGE ( 'NONE', *, *, #10069, .T. ) ;
#6931 = B_SPLINE_CURVE_WITH_KNOTS ( 'NONE', 3,
 ( #10370, #1683, #6624, #10432, #4605, #2826, #5565, #12408, #859, #10495, #9621, #11455, #3705, #9558, #3771, #6690, #2574, #5507 ),
 .UNSPECIFIED., .F., .F.,
 ( 4, 2, 2, 2, 2, 2, 2, 2, 4 ),
 ( 0.007846355738354819295, 0.008826646719051039688, 0.009806937699747258347, 0.01078722868044347874, 0.01176751966113969913, 0.01274781064183591779, 0.01372810162253213818, 0.01470839260322835684, 0.01568868358392457724 ),
 .UNSPECIFIED. ) ;
#6932 = VERTEX_POINT ( 'NONE', #8602 ) ;
#6933 = CARTESIAN_POINT ( 'NONE',  ( 9.469886687176911622, 16.77055699046783843, 26.35017345530262745 ) ) ;
#6934 = LINE ( 'NONE', #7895, #965 ) ;
#6935 = LINE ( 'NONE', #6877, #11215 ) ;
#6936 = CARTESIAN_POINT ( 'NONE',  ( 29.77500000054622831, 20.00000000000000355, 98.07665518445361386 ) ) ;
#6937 = CARTESIAN_POINT ( 'NONE',  ( 29.17500000054622333, 26.19570976099943493, 86.29171490190961435 ) ) ;
#6938 = AXIS2_PLACEMENT_3D ( 'NONE', #5715, #5473, #8501 ) ;
#6939 = CARTESIAN_POINT ( 'NONE',  ( -3.975160125666882482, 53.05023972334481641, 27.71699044896146447 ) ) ;
#6940 = CARTESIAN_POINT ( 'NONE',  ( -9.096797777268143648, 24.16610281865074583, 18.92797567942162829 ) ) ;
#6941 = CARTESIAN_POINT ( 'NONE',  ( 34.72841614740047333, 22.00000000000000000, 152.2284161474004520 ) ) ;
#6942 = ORIENTED_EDGE ( 'NONE', *, *, #6111, .F. ) ;
#6943 = CARTESIAN_POINT ( 'NONE',  ( 49.17500000054622689, 26.19570976099943849, 86.29171490190961435 ) ) ;
#6944 = CARTESIAN_POINT ( 'NONE',  ( 3.968701803879573831, 53.04568146648268367, -24.68320166897649770 ) ) ;
#6945 = DIRECTION ( 'NONE',  ( 0.000000000000000000, 0.000000000000000000, -1.000000000000000000 ) ) ;
#6946 = ORIENTED_EDGE ( 'NONE', *, *, #5725, .T. ) ;
#6947 = ADVANCED_FACE ( 'NONE', ( #10499 ), #12534, .F. ) ;
#6948 = CARTESIAN_POINT ( 'NONE',  ( 122.0000000000000000, 5.035999999999999588, 0.000000000000000000 ) ) ;
#6949 = ORIENTED_EDGE ( 'NONE', *, *, #11393, .T. ) ;
#6950 = FACE_OUTER_BOUND ( 'NONE', #2112, .T. ) ;
#6951 = CARTESIAN_POINT ( 'NONE',  ( -3.245616027290198602, 10.51897860477085622, -24.79588311023535852 ) ) ;
#6952 = AXIS2_PLACEMENT_3D ( 'NONE', #7984, #4105, #9954 ) ;
#6953 = CARTESIAN_POINT ( 'NONE',  ( 0.000000000000000000, -4.262400816306111331E-15, -28.00000000000000355 ) ) ;
#6954 = CARTESIAN_POINT ( 'NONE',  ( 3.061565168526138680E-15, 55.00000000000000000, 25.00000000000000000 ) ) ;
#6955 = CARTESIAN_POINT ( 'NONE',  ( 7.621040678280055047, 26.47631533951529192, 87.00314373824969039 ) ) ;
#6956 = CARTESIAN_POINT ( 'NONE',  ( 4.967203680380478659, 49.34177296812513447, -24.50165547367289065 ) ) ;
#6957 = CIRCLE ( 'NONE', #885, 6.000000000000003553 ) ;
#6958 = DIRECTION ( 'NONE',  ( 0.000000000000000000, 0.000000000000000000, 1.000000000000000000 ) ) ;
#6959 = DIRECTION ( 'NONE',  ( 0.000000000000000000, 0.000000000000000000, 1.000000000000000000 ) ) ;
#6960 = CARTESIAN_POINT ( 'NONE',  ( 10.00000000000000355, 20.00000000000000355, 109.9999999999999858 ) ) ;
#6961 = CARTESIAN_POINT ( 'NONE',  ( 40.37500000054622973, 13.07298590277314432, 88.54243821818161564 ) ) ;
#6962 =( GEOMETRIC_REPRESENTATION_CONTEXT ( 3 ) GLOBAL_UNCERTAINTY_ASSIGNED_CONTEXT ( ( #4024 ) ) GLOBAL_UNIT_ASSIGNED_CONTEXT ( ( #12066, #7236, #4442 ) ) REPRESENTATION_CONTEXT ( 'NONE', 'WORKASPACE' ) );
#6963 = CARTESIAN_POINT ( 'NONE',  ( 4.337416167900176589, 47.49133373970335015, 20.54801971059908894 ) ) ;
#6964 = EDGE_LOOP ( 'NONE', ( #11747, #8178, #4208, #2427 ) ) ;
#6965 = CARTESIAN_POINT ( 'NONE',  ( 37.65000000109246514, 20.00000000000000355, 98.29316153445363113 ) ) ;
#6966 = EDGE_CURVE ( 'NONE', #4253, #2928, #1934, .T. ) ;
#6967 = SHAPE_DEFINITION_REPRESENTATION ( #9146, #6122 ) ;
#6968 = AXIS2_PLACEMENT_3D ( 'NONE', #5552, #10294, #12209 ) ;
#6969 = CARTESIAN_POINT ( 'NONE',  ( 28.99999999999998934, 20.00000000000000355, 83.29316153445364534 ) ) ;
#6970 = CARTESIAN_POINT ( 'NONE',  ( 0.000000000000000000, 20.00000000000000355, -28.00000000000000711 ) ) ;
#6971 = EDGE_CURVE ( 'NONE', #12368, #667, #1293, .T. ) ;
#6972 = CARTESIAN_POINT ( 'NONE',  ( 32.17500000054622689, 13.07298590277314254, 93.04388485072563242 ) ) ;
#6973 = CARTESIAN_POINT ( 'NONE',  ( 21.07500000054622191, 24.28113015263587471, 84.90069139318163138 ) ) ;
#6974 = CARTESIAN_POINT ( 'NONE',  ( 24.09999999999998366, 17.56310227825320425, 98.29316153445363113 ) ) ;
#6975 = DIRECTION ( 'NONE',  ( -0.000000000000000000, -0.000000000000000000, 1.000000000000000000 ) ) ;
#6976 = CARTESIAN_POINT ( 'NONE',  ( 26.37500000054622973, 13.07298590277314432, 88.54243821818161564 ) ) ;
#6977 = ORIENTED_EDGE ( 'NONE', *, *, #1010, .T. ) ;
#6978 = CARTESIAN_POINT ( 'NONE',  ( 0.000000000000000000, 0.000000000000000000, 0.000000000000000000 ) ) ;
#6979 = SURFACE_STYLE_USAGE ( .BOTH. , #1158 ) ;
#6980 = ORIENTED_EDGE ( 'NONE', *, *, #2474, .F. ) ;
#6981 = VECTOR ( 'NONE', #4097, 1000.000000000000114 ) ;
#6982 = CARTESIAN_POINT ( 'NONE',  ( -2.000000000000015543, 20.00000000000000355, 83.29316153445364534 ) ) ;
#6983 = ADVANCED_FACE ( 'NONE', ( #7528 ), #108, .T. ) ;
#6984 = ORIENTED_EDGE ( 'NONE', *, *, #7346, .T. ) ;
#6985 = DIRECTION ( 'NONE',  ( -0.000000000000000000, -0.000000000000000000, 1.000000000000000000 ) ) ;
#6986 = CARTESIAN_POINT ( 'NONE',  ( 27.49999999999999645, 20.00000000000000355, 169.9999999999999716 ) ) ;
#6987 = CARTESIAN_POINT ( 'NONE',  ( 38.87500000054622262, 20.00000000000000355, 83.50966788445364841 ) ) ;
#6988 = DIRECTION ( 'NONE',  ( 0.000000000000000000, 0.000000000000000000, 1.000000000000000000 ) ) ;
#6989 = EDGE_CURVE ( 'NONE', #2550, #2108, #74, .T. ) ;
#6990 = CARTESIAN_POINT ( 'NONE',  ( -5.000000000000000000, 49.66965428365661239, -27.54995462791182348 ) ) ;
#6991 = CARTESIAN_POINT ( 'NONE',  ( 42.69999999999998863, 13.62011893735971135, 86.15790661882942914 ) ) ;
#6992 = CARTESIAN_POINT ( 'NONE',  ( 45.39999999999999147, 27.13292387221364876, 88.47553407664153724 ) ) ;
#6993 = VERTEX_POINT ( 'NONE', #298 ) ;
#6994 = ADVANCED_FACE ( 'NONE', ( #8728 ), #12034, .F. ) ;
#6995 = CARTESIAN_POINT ( 'NONE',  ( 32.85000000109246088, 24.40838939219355197, 84.72553407664153724 ) ) ;
#6996 = CARTESIAN_POINT ( 'NONE',  ( 4.967203680380478659, 49.34177296812513447, -24.50165547367289065 ) ) ;
#6997 = ORIENTED_EDGE ( 'NONE', *, *, #6685, .T. ) ;
#6998 = EDGE_CURVE ( 'NONE', #9685, #481, #1082, .T. ) ;
#6999 = CARTESIAN_POINT ( 'NONE',  ( 4.999999999999999112, 40.00000000000000000, 121.2488769092545198 ) ) ;
#7000 = AXIS2_PLACEMENT_3D ( 'NONE', #9753, #44, #2832 ) ;
#7001 = ORIENTED_EDGE ( 'NONE', *, *, #9929, .T. ) ;
#7002 = LINE ( 'NONE', #10873, #2225 ) ;
#7003 = CIRCLE ( 'NONE', #7207, 9.000000000000000000 ) ;
#7004 = EDGE_CURVE ( 'NONE', #10467, #3111, #2466, .T. ) ;
#7005 = CARTESIAN_POINT ( 'NONE',  ( -50.00000000000001421, 20.00000000000000000, 145.0000000000000000 ) ) ;
#7006 = CARTESIAN_POINT ( 'NONE',  ( -50.00000000000001421, 92.00000000000000000, 69.99999999999998579 ) ) ;
#7007 = PRODUCT_DEFINITION_CONTEXT ( 'detailed design', #5622, 'design' ) ;
#7008 = CARTESIAN_POINT ( 'NONE',  ( 30.77500000054622831, 20.00000000000000355, 83.50966788445364841 ) ) ;
#7009 = CARTESIAN_POINT ( 'NONE',  ( 33.57500000054622546, 26.19570976099943493, 95.29460816699764791 ) ) ;
#7010 = CARTESIAN_POINT ( 'NONE',  ( 6.000000000000000000, -2.919948986426538884, -5.057499999999997442 ) ) ;
#7011 = CARTESIAN_POINT ( 'NONE',  ( 10.00000000000000000, 20.65873750777989670, -26.15339366124403497 ) ) ;
#7012 = CARTESIAN_POINT ( 'NONE',  ( 33.75000000109245946, 17.56310227825320425, 98.29316153445363113 ) ) ;
#7013 = VERTEX_POINT ( 'NONE', #42 ) ;
#7014 = CARTESIAN_POINT ( 'NONE',  ( 48.35000000109246798, 13.62011893735971135, 86.15790661882942914 ) ) ;
#7015 = ORIENTED_EDGE ( 'NONE', *, *, #8147, .T. ) ;
#7016 = CARTESIAN_POINT ( 'NONE',  ( 12.00000000000000355, 0.000000000000000000, 0.000000000000000000 ) ) ;
#7017 = ORIENTED_EDGE ( 'NONE', *, *, #8043, .F. ) ;
#7018 = LINE ( 'NONE', #8924, #6981 ) ;
#7019 = CARTESIAN_POINT ( 'NONE',  ( -10.00000000000000355, 20.00000000000000355, -22.91287847477919826 ) ) ;
#7020 = VECTOR ( 'NONE', #9381, 1000.000000000000000 ) ;
#7021 = DIRECTION ( 'NONE',  ( -1.000000000000000000, -0.000000000000000000, -0.000000000000000000 ) ) ;
#7022 = CARTESIAN_POINT ( 'NONE',  ( 6.629604629042566089, 27.48664723726108505, 90.27812524726596166 ) ) ;
#7023 = CARTESIAN_POINT ( 'NONE',  ( 2.502435999373153308, 45.66817884423451801, -24.87486459250430926 ) ) ;
#7024 = DIRECTION ( 'NONE',  ( 0.000000000000000000, 0.000000000000000000, -1.000000000000000000 ) ) ;
#7025 = CARTESIAN_POINT ( 'NONE',  ( -3.306282206746268937, 53.76494240372728939, 20.73941076293121810 ) ) ;
#7026 = DIRECTION ( 'NONE',  ( 0.000000000000000000, 0.5000000000000012212, 0.8660254037844379305 ) ) ;
#7027 = CARTESIAN_POINT ( 'NONE',  ( 42.87500000054622973, 22.36655054427230382, 83.50966788445364841 ) ) ;
#7028 = CARTESIAN_POINT ( 'NONE',  ( -27.49999999999999645, 27.49999999999999645, 145.0000000000000000 ) ) ;
#7029 = ORIENTED_EDGE ( 'NONE', *, *, #235, .T. ) ;
#7030 = DIRECTION ( 'NONE',  ( 0.000000000000000000, -0.4999999999999990008, 0.8660254037844391517 ) ) ;
#7031 = AXIS2_PLACEMENT_3D ( 'NONE', #1847, #5486, #4775 ) ;
#7032 = ADVANCED_FACE ( 'NONE', ( #10951 ), #1073, .F. ) ;
#7033 = CARTESIAN_POINT ( 'NONE',  ( 22.77500000054622120, 17.63344945572770328, 83.50966788445364841 ) ) ;
#7034 = CARTESIAN_POINT ( 'NONE',  ( 41.77500000054621410, 22.36655054427230027, 98.07665518445361386 ) ) ;
#7035 = CARTESIAN_POINT ( 'NONE',  ( 35.07500000054622546, 26.19570976099943849, 86.29171490190961435 ) ) ;
#7036 = CARTESIAN_POINT ( 'NONE',  ( 20.97500000054622404, 22.36655054427230382, 83.50966788445364841 ) ) ;
#7037 = CARTESIAN_POINT ( 'NONE',  ( 20.89999999999999147, 17.56310227825321135, 83.29316153445363113 ) ) ;
#7038 = CARTESIAN_POINT ( 'NONE',  ( -5.000000000000000000, 50.00000000000000000, -28.00000000000000711 ) ) ;
#7039 = CARTESIAN_POINT ( 'NONE',  ( 25.97500000054622760, 15.71886984736413417, 96.68563167572563088 ) ) ;
#7040 = ORIENTED_EDGE ( 'NONE', *, *, #5312, .F. ) ;
#7041 = CARTESIAN_POINT ( 'NONE',  ( 0.000000000000000000, 2.342598717236900718, -4.057500000000001883 ) ) ;
#7042 = ORIENTED_EDGE ( 'NONE', *, *, #11233, .T. ) ;
#7043 = VERTEX_POINT ( 'NONE', #8413 ) ;
#7044 = CARTESIAN_POINT ( 'NONE',  ( -20.27158385259952667, 18.00000000000000355, 152.2284161474004520 ) ) ;
#7045 = ORIENTED_EDGE ( 'NONE', *, *, #11312, .T. ) ;
#7046 = CARTESIAN_POINT ( 'NONE',  ( -4.968205859249467338, 50.65222807605660904, -24.50145347565533882 ) ) ;
#7047 = CARTESIAN_POINT ( 'NONE',  ( 41.37500000054622262, 27.65831843345427998, 90.79316153445363113 ) ) ;
#7048 = DIRECTION ( 'NONE',  ( 0.000000000000000000, 0.000000000000000000, 1.000000000000000000 ) ) ;
#7049 = CARTESIAN_POINT ( 'NONE',  ( 26.19999999999998863, 15.59161060780645691, 96.86078899226572503 ) ) ;
#7050 = CARTESIAN_POINT ( 'NONE',  ( 38.67500000054622689, 15.71886984736413773, 84.90069139318163138 ) ) ;
#7051 = CARTESIAN_POINT ( 'NONE',  ( 44.59999999999998721, 12.86707612778636012, 88.47553407664152303 ) ) ;
#7052 = EDGE_CURVE ( 'NONE', #5467, #1996, #8926, .T. ) ;
#7053 = CARTESIAN_POINT ( 'NONE',  ( 48.07500000054623257, 13.80429023900056507, 95.29460816699764791 ) ) ;
#7054 = ORIENTED_EDGE ( 'NONE', *, *, #471, .T. ) ;
#7055 = CARTESIAN_POINT ( 'NONE',  ( 24.15000000109245804, 12.11403331821300533, 90.79316153445363113 ) ) ;
#7056 = LINE ( 'NONE', #9985, #5488 ) ;
#7057 = ORIENTED_EDGE ( 'NONE', *, *, #1954, .F. ) ;
#7058 = VECTOR ( 'NONE', #10195, 1000.000000000000000 ) ;
#7059 = CARTESIAN_POINT ( 'NONE',  ( 0.000000000000000000, 0.000000000000000000, 169.9999999999999716 ) ) ;
#7060 = ORIENTED_EDGE ( 'NONE', *, *, #11108, .F. ) ;
#7061 = CIRCLE ( 'NONE', #995, 6.599999999999998757 ) ;
#7062 = FACE_OUTER_BOUND ( 'NONE', #6285, .T. ) ;
#7063 = CARTESIAN_POINT ( 'NONE',  ( 40.99999999999998579, 20.00000000000000355, 83.29316153445364534 ) ) ;
#7064 = CARTESIAN_POINT ( 'NONE',  ( 38.65000000109246514, 20.00000000000000355, 83.29316153445364534 ) ) ;
#7065 = VECTOR ( 'NONE', #10209, 999.9999999999998863 ) ;
#7066 = CARTESIAN_POINT ( 'NONE',  ( 27.57500000054622902, 24.28113015263587116, 96.68563167572563088 ) ) ;
#7067 = CARTESIAN_POINT ( 'NONE',  ( 28.37500000054622618, 12.34168156654572535, 90.79316153445363113 ) ) ;
#7068 = EDGE_CURVE ( 'NONE', #7957, #7937, #6196, .T. ) ;
#7069 = FACE_OUTER_BOUND ( 'NONE', #10778, .T. ) ;
#7070 = DIRECTION ( 'NONE',  ( -1.000000000000000000, -0.000000000000000000, -0.000000000000000000 ) ) ;
#7071 = CARTESIAN_POINT ( 'NONE',  ( -0.6591801397249409389, 45.03285316749953182, 24.99337097521990003 ) ) ;
#7072 = VERTEX_POINT ( 'NONE', #429 ) ;
#7073 = CARTESIAN_POINT ( 'NONE',  ( 1.620000493755592075, 54.74147302055352071, -24.94927790585931504 ) ) ;
#7074 = CARTESIAN_POINT ( 'NONE',  ( 6.000000000000000000, 5.839897972853064445, -8.673617379884035472E-15 ) ) ;
#7075 = ORIENTED_EDGE ( 'NONE', *, *, #12541, .F. ) ;
#7076 = DIRECTION ( 'NONE',  ( -1.000000000000000000, -0.000000000000000000, -0.000000000000000000 ) ) ;
#7077 = ADVANCED_FACE ( 'NONE', ( #613 ), #4478, .F. ) ;
#7078 = EDGE_LOOP ( 'NONE', ( #1065, #4226, #4730, #9116 ) ) ;
#7079 = CARTESIAN_POINT ( 'NONE',  ( -9.481501190889247255, 16.75403870714897536, -23.13387092261990574 ) ) ;
#7080 = AXIS2_PLACEMENT_3D ( 'NONE', #6485, #5420, #9291 ) ;
#7081 = CARTESIAN_POINT ( 'NONE',  ( 0.6000000000000033085, 0.000000000000000000, 0.000000000000000000 ) ) ;
#7082 = PRESENTATION_STYLE_ASSIGNMENT (( #1383 ) ) ;
#7083 = CARTESIAN_POINT ( 'NONE',  ( 9.794823006331467852, 22.03034270180912557, 83.56881077602001540 ) ) ;
#7084 = LINE ( 'NONE', #10965, #9505 ) ;
#7085 = CARTESIAN_POINT ( 'NONE',  ( -3.302172444309792620, 46.23123523635531740, -24.78206517003335208 ) ) ;
#7086 = CARTESIAN_POINT ( 'NONE',  ( -3.050155127176687575, 53.97520719309672188, 20.77909757380590250 ) ) ;
#7087 = DIRECTION ( 'NONE',  ( -0.000000000000000000, -1.000000000000000000, -0.000000000000000000 ) ) ;
#7088 = CARTESIAN_POINT ( 'NONE',  ( 42.67500000054623399, 17.63344945572770328, 83.50966788445364841 ) ) ;
#7089 = CARTESIAN_POINT ( 'NONE',  ( -4.838879514055022923, 48.69911239754581089, -24.52732196506755713 ) ) ;
#7090 = EDGE_LOOP ( 'NONE', ( #3077, #7850, #1365, #6162, #10932 ) ) ;
#7091 = CARTESIAN_POINT ( 'NONE',  ( -3.973554925899839052, 53.05255087154787219, 24.68288788663009825 ) ) ;
#7092 = CIRCLE ( 'NONE', #9730, 5.057500000000000107 ) ;
#7093 = CARTESIAN_POINT ( 'NONE',  ( 22.57500000054622546, 13.80429023900056684, 86.29171490190961435 ) ) ;
#7094 = CARTESIAN_POINT ( 'NONE',  ( 41.87500000054622262, 20.00000000000000355, 98.07665518445361386 ) ) ;
#7095 = CARTESIAN_POINT ( 'NONE',  ( 31.67500000054622333, 22.36655054427230027, 98.07665518445361386 ) ) ;
#7096 = CARTESIAN_POINT ( 'NONE',  ( 0.6581862696184550554, 10.01618719080246578, -24.99351150626209161 ) ) ;
#7097 = CARTESIAN_POINT ( 'NONE',  ( 44.75000000109246656, 22.43689772174682417, 83.29316153445364534 ) ) ;
#7098 = LINE ( 'NONE', #7038, #6269 ) ;
#7099 = CARTESIAN_POINT ( 'NONE',  ( 25.17500000054623044, 26.92701409722686634, 88.54243821818162985 ) ) ;
#7100 = VERTEX_POINT ( 'NONE', #4357 ) ;
#7101 = CIRCLE ( 'NONE', #8726, 9.000000000000000000 ) ;
#7102 = ADVANCED_FACE ( 'NONE', ( #8353 ), #688, .F. ) ;
#7103 = PRODUCT_DEFINITION_SHAPE ( 'NONE', 'NONE',  #12545 ) ;
#7104 = CARTESIAN_POINT ( 'NONE',  ( 33.25000000109245946, 27.13292387221364876, 93.11078899226573924 ) ) ;
#7105 = ORIENTED_EDGE ( 'NONE', *, *, #3037, .F. ) ;
#7106 = ORIENTED_EDGE ( 'NONE', *, *, #5690, .F. ) ;
#7107 = ADVANCED_FACE ( 'NONE', ( #3523 ), #672, .T. ) ;
#7108 = LINE ( 'NONE', #8254, #8529 ) ;
#7109 = ORIENTED_EDGE ( 'NONE', *, *, #7052, .T. ) ;
#7110 = DIRECTION ( 'NONE',  ( 0.000000000000000000, 0.000000000000000000, 1.000000000000000000 ) ) ;
#7111 = EDGE_CURVE ( 'NONE', #3052, #1035, #3114, .T. ) ;
#7112 = AXIS2_PLACEMENT_3D ( 'NONE', #9691, #6631, #45 ) ;
#7113 = CARTESIAN_POINT ( 'NONE',  ( 40.07500000054623257, 15.71886984736413417, 96.68563167572563088 ) ) ;
#7114 = DIRECTION ( 'NONE',  ( 0.000000000000000000, 0.000000000000000000, 1.000000000000000000 ) ) ;
#7115 = CARTESIAN_POINT ( 'NONE',  ( -3.303799404834185438, 46.23288169458685104, -27.80537610472761045 ) ) ;
#7116 = CARTESIAN_POINT ( 'NONE',  ( 38.47500000054622404, 13.07298590277314432, 88.54243821818161564 ) ) ;
#7117 = CARTESIAN_POINT ( 'NONE',  ( 38.99999999999998579, 20.00000000000000355, 83.29316153445364534 ) ) ;
#7118 = CARTESIAN_POINT ( 'NONE',  ( 48.77500000054622831, 20.00000000000000355, 83.50966788445364841 ) ) ;
#7119 = ORIENTED_EDGE ( 'NONE', *, *, #418, .F. ) ;
#7120 =( GEOMETRIC_REPRESENTATION_CONTEXT ( 3 ) GLOBAL_UNCERTAINTY_ASSIGNED_CONTEXT ( ( #11655 ) ) GLOBAL_UNIT_ASSIGNED_CONTEXT ( ( #362, #12213, #2563 ) ) REPRESENTATION_CONTEXT ( 'NONE', 'WORKASPACE' ) );
#7121 = CARTESIAN_POINT ( 'NONE',  ( 23.45000000109246585, 24.40838939219354842, 96.86078899226572503 ) ) ;
#7122 = CARTESIAN_POINT ( 'NONE',  ( -4.493559251511619834, 47.78304274923282691, 24.59317321405577772 ) ) ;
#7123 = EDGE_LOOP ( 'NONE', ( #6438, #12062, #3001, #7579 ) ) ;
#7124 = PLANE ( 'NONE',  #2447 ) ;
#7125 = ORIENTED_EDGE ( 'NONE', *, *, #8549, .F. ) ;
#7126 = EDGE_CURVE ( 'NONE', #9969, #2800, #12037, .T. ) ;
#7127 = CARTESIAN_POINT ( 'NONE',  ( 36.15000000109245804, 12.11403331821300533, 90.79316153445363113 ) ) ;
#7128 = CARTESIAN_POINT ( 'NONE',  ( -7.994063978020062912E-22, 10.00000000000000000, -21.00000000000000000 ) ) ;
#7129 = CARTESIAN_POINT ( 'NONE',  ( 33.47500000054623115, 26.19570976099943493, 95.29460816699764791 ) ) ;
#7130 = CARTESIAN_POINT ( 'NONE',  ( 33.17500000054622689, 26.19570976099943493, 86.29171490190961435 ) ) ;
#7131 = EDGE_CURVE ( 'NONE', #2352, #12211, #9131, .T. ) ;
#7132 = CARTESIAN_POINT ( 'NONE',  ( 9.933961117401199914, 21.32149700181756558, 26.17890995529624476 ) ) ;
#7133 = CARTESIAN_POINT ( 'NONE',  ( 21.75000000109246656, 17.56310227825320425, 98.29316153445363113 ) ) ;
#7134 = ORIENTED_EDGE ( 'NONE', *, *, #3099, .T. ) ;
#7135 = CARTESIAN_POINT ( 'NONE',  ( 47.05000000109247082, 27.13292387221364876, 88.47553407664153724 ) ) ;
#7136 = VERTEX_POINT ( 'NONE', #3768 ) ;
#7137 = CARTESIAN_POINT ( 'NONE',  ( 0.000000000000000000, -5.839897972853063557, 6.938893903907228378E-15 ) ) ;
#7138 = VERTEX_POINT ( 'NONE', #3835 ) ;
#7139 = CARTESIAN_POINT ( 'NONE',  ( -10.00000000000000355, 19.66998333124466214, -22.91287847477919826 ) ) ;
#7140 = CARTESIAN_POINT ( 'NONE',  ( 0.6581862696184550554, 10.01618719080246578, -24.99351150626209161 ) ) ;
#7141 =( BOUNDED_CURVE ( )  B_SPLINE_CURVE ( 2, ( #10697, #8739, #52, #9761, #4933, #8801, #6894, #7918, #10759, #8866, #9824 ),
 .UNSPECIFIED., .F., .F. ) 
 B_SPLINE_CURVE_WITH_KNOTS ( ( 3, 2, 2, 2, 2, 3 ),
 ( 0.3999999999999998557, 0.4066666666666665098, 0.4133333333333332194, 0.4199999999999998734, 0.4266666666666666385, 0.4333333333333332926 ),
 .UNSPECIFIED. ) 
 CURVE ( )  GEOMETRIC_REPRESENTATION_ITEM ( )  RATIONAL_B_SPLINE_CURVE ( ( 1.000000000000001332, 0.9510565162951524210, 1.000000000000000000, 0.9510565162951535312, 1.000000000000000000, 0.9510565162951535312, 1.000000000000000000, 0.9510565162951535312, 1.000000000000000000, 0.9510565162951539753, 0.9999999999999995559 ) ) 
 REPRESENTATION_ITEM ( '' )  );
#7142 = LINE ( 'NONE', #11019, #10071 ) ;
#7143 = LINE ( 'NONE', #493, #1564 ) ;
#7144 = EDGE_CURVE ( 'NONE', #110, #8158, #12466, .T. ) ;
#7145 = DIRECTION ( 'NONE',  ( 0.000000000000000000, 0.5000000000000009992, 0.8660254037844380415 ) ) ;
#7146 = DIRECTION ( 'NONE',  ( -0.000000000000000000, 0.000000000000000000, 1.000000000000000000 ) ) ;
#7147 = DIRECTION ( 'NONE',  ( 0.000000000000000000, 0.000000000000000000, -1.000000000000000000 ) ) ;
#7148 = CYLINDRICAL_SURFACE ( 'NONE', #11619, 7.500000000000000000 ) ;
#7149 = CARTESIAN_POINT ( 'NONE',  ( -4.556456226338131188, 47.93475174319672760, 27.62684759756936970 ) ) ;
#7150 = APPLICATION_CONTEXT ( 'automotive_design' ) ;
#7151 = LINE ( 'NONE', #8113, #7505 ) ;
#7152 = VERTEX_POINT ( 'NONE', #1804 ) ;
#7153 = EDGE_CURVE ( 'NONE', #4738, #10817, #1305, .T. ) ;
#7154 = DIRECTION ( 'NONE',  ( -0.000000000000000000, -1.000000000000000000, -0.000000000000000000 ) ) ;
#7155 = CARTESIAN_POINT ( 'NONE',  ( 28.49999999999998579, 12.11403331821300533, 90.79316153445363113 ) ) ;
#7156 = CARTESIAN_POINT ( 'NONE',  ( 43.37500000054622973, 27.65831843345427998, 90.79316153445363113 ) ) ;
#7157 = VECTOR ( 'NONE', #9453, 1000.000000000000000 ) ;
#7158 = CARTESIAN_POINT ( 'NONE',  ( 26.37500000054622973, 13.07298590277314432, 88.54243821818161564 ) ) ;
#7159 = CARTESIAN_POINT ( 'NONE',  ( 9.621890409868294469, 17.26583415636358154, 97.78138982115301303 ) ) ;
#7160 = FACE_OUTER_BOUND ( 'NONE', #12382, .T. ) ;
#7161 = CARTESIAN_POINT ( 'NONE',  ( 34.99999999999999289, 20.00000000000000355, 170.0000119999999697 ) ) ;
#7162 = DIRECTION ( 'NONE',  ( 1.000000000000000000, 0.000000000000000000, 0.000000000000000000 ) ) ;
#7163 = CARTESIAN_POINT ( 'NONE',  ( 23.97500000054623115, 15.71886984736413417, 96.68563167572563088 ) ) ;
#7164 = ORIENTED_EDGE ( 'NONE', *, *, #7927, .T. ) ;
#7165 = CARTESIAN_POINT ( 'NONE',  ( 32.85000000109246088, 24.40838939219355197, 84.72553407664153724 ) ) ;
#7166 = EDGE_LOOP ( 'NONE', ( #11657, #9689, #10439, #8241 ) ) ;
#7167 = LINE ( 'NONE', #5154, #3057 ) ;
#7168 = B_SPLINE_CURVE_WITH_KNOTS ( 'NONE', 3,
 ( #9802, #5107, #352, #4216, #6179, #1366, #2183, #9104, #4018, #11763, #4149, #8088, #6055, #11895, #3199, #5233, #1112, #11064, #6933, #2116, #5992, #10349, #1665, #717 ),
 .UNSPECIFIED., .F., .F.,
 ( 4, 2, 2, 2, 2, 2, 2, 2, 2, 2, 2, 4 ),
 ( 0.04728207046791076812, 0.04925237334111622067, 0.05023752477771894348, 0.05122267621432167323, 0.05220782765092439603, 0.05319297908752712578, 0.05516328196073257140, 0.05713358483393803089, 0.05910388770714347650, 0.06008903914374620625, 0.06107419058034893600, 0.06304449345355438161 ),
 .UNSPECIFIED. ) ;
#7169 = ORIENTED_EDGE ( 'NONE', *, *, #10215, .F. ) ;
#7170 = VECTOR ( 'NONE', #5109, 1000.000000000000000 ) ;
#7171 = CARTESIAN_POINT ( 'NONE',  ( 0.000000000000000000, 0.000000000000000000, 0.000000000000000000 ) ) ;
#7172 = VECTOR ( 'NONE', #10881, 1000.000000000000000 ) ;
#7173 = CARTESIAN_POINT ( 'NONE',  ( 34.47500000054622404, 13.07298590277314432, 88.54243821818161564 ) ) ;
#7174 = CARTESIAN_POINT ( 'NONE',  ( -5.000000000000000000, 50.00000000000000000, -24.49489742783178059 ) ) ;
#7175 = CARTESIAN_POINT ( 'NONE',  ( 26.69999999999998508, 13.62011893735970958, 86.15790661882942914 ) ) ;
#7176 = CARTESIAN_POINT ( 'NONE',  ( 34.57500000054621125, 13.80429023900056684, 86.29171490190961435 ) ) ;
#7177 = CARTESIAN_POINT ( 'NONE',  ( 39.29999999999999005, 26.37988106264029398, 86.15790661882942914 ) ) ;
#7178 = CARTESIAN_POINT ( 'NONE',  ( 42.77500000054622831, 20.00000000000000355, 83.50966788445364841 ) ) ;
#7179 = VERTEX_POINT ( 'NONE', #856 ) ;
#7180 = VECTOR ( 'NONE', #8336, 1000.000000000000000 ) ;
#7181 = CARTESIAN_POINT ( 'NONE',  ( 26.95000000109246585, 26.37988106264029398, 86.15790661882942914 ) ) ;
#7182 = CARTESIAN_POINT ( 'NONE',  ( -4.967261190099589108, 49.34148114543111774, 24.50164489405593571 ) ) ;
#7183 = ORIENTED_EDGE ( 'NONE', *, *, #1269, .F. ) ;
#7184 = CARTESIAN_POINT ( 'NONE',  ( -9.918969497010245107, 21.31253892522589055, 26.18425576506515640 ) ) ;
#7185 = ORIENTED_EDGE ( 'NONE', *, *, #6000, .T. ) ;
#7186 = CARTESIAN_POINT ( 'NONE',  ( 25.35000000109246443, 26.37988106264029398, 95.42841645007781892 ) ) ;
#7187 = CARTESIAN_POINT ( 'NONE',  ( 4.555810879675650682, 47.93324276400543482, -27.62695503246266071 ) ) ;
#7188 = COLOUR_RGB ( '',0.7921568627450980005, 0.8196078431372548767, 0.9333333333333333481 ) ;
#7189 = DIRECTION ( 'NONE',  ( 0.000000000000000000, 0.000000000000000000, 1.000000000000000000 ) ) ;
#7190 = EDGE_CURVE ( 'NONE', #4057, #3460, #2760, .T. ) ;
#7191 = CARTESIAN_POINT ( 'NONE',  ( 30.97500000054622760, 24.28113015263587471, 84.90069139318163138 ) ) ;
#7192 = CARTESIAN_POINT ( 'NONE',  ( 24.67500000054622689, 15.71886984736413773, 84.90069139318163138 ) ) ;
#7193 = DIRECTION ( 'NONE',  ( 0.000000000000000000, -1.000000000000000000, 0.000000000000000000 ) ) ;
#7194 = LINE ( 'NONE', #9237, #1983 ) ;
#7195 = ORIENTED_EDGE ( 'NONE', *, *, #8392, .T. ) ;
#7196 = EDGE_CURVE ( 'NONE', #4253, #7136, #9556, .T. ) ;
#7197 = CARTESIAN_POINT ( 'NONE',  ( 47.15000000109245804, 27.88596668178699645, 90.79316153445363113 ) ) ;
#7198 = ORIENTED_EDGE ( 'NONE', *, *, #4084, .T. ) ;
#7199 = CARTESIAN_POINT ( 'NONE',  ( 47.39999999999999147, 27.13292387221364876, 88.47553407664153724 ) ) ;
#7200 = ORIENTED_EDGE ( 'NONE', *, *, #6809, .F. ) ;
#7201 = CARTESIAN_POINT ( 'NONE',  ( -7.511663825336949429, 13.39091019075763533, -19.61183490434176235 ) ) ;
#7202 = CARTESIAN_POINT ( 'NONE',  ( -0.6600000499078774174, 29.98375368882421910, 24.99348755773349140 ) ) ;
#7203 = CARTESIAN_POINT ( 'NONE',  ( 5.000000000000000000, 0.000000000000000000, 0.000000000000000000 ) ) ;
#7204 = EDGE_CURVE ( 'NONE', #5738, #5882, #8596, .T. ) ;
#7205 = PRESENTATION_STYLE_ASSIGNMENT (( #12162 ) ) ;
#7206 = PRODUCT_DEFINITION_SHAPE ( 'NONE', 'NONE',  #1691 ) ;
#7207 = AXIS2_PLACEMENT_3D ( 'NONE', #8546, #12413, #6630 ) ;
#7208 = CARTESIAN_POINT ( 'NONE',  ( 0.000000000000000000, -2.919948986426538884, -5.057499999999997442 ) ) ;
#7209 = DIRECTION ( 'NONE',  ( 0.000000000000000000, 0.000000000000000000, -1.000000000000000000 ) ) ;
#7210 = EDGE_CURVE ( 'NONE', #3844, #2550, #9680, .T. ) ;
#7211 = CARTESIAN_POINT ( 'NONE',  ( -2.625488409636790088, 10.34519051174632764, 20.83765690359550860 ) ) ;
#7212 = DIRECTION ( 'NONE',  ( -0.000000000000000000, -0.000000000000000000, 1.000000000000000000 ) ) ;
#7213 = CARTESIAN_POINT ( 'NONE',  ( 3.061617454482527662E-15, 30.00000000000001066, 25.00000000000000000 ) ) ;
#7214 = CARTESIAN_POINT ( 'NONE',  ( -0.3266958997752330562, 45.00000000000001421, -25.00000000000000355 ) ) ;
#7215 = ORIENTED_EDGE ( 'NONE', *, *, #985, .T. ) ;
#7216 =( BOUNDED_CURVE ( )  B_SPLINE_CURVE ( 3, ( #2681, #4522, #7377, #2553 ),
 .UNSPECIFIED., .F., .F. ) 
 B_SPLINE_CURVE_WITH_KNOTS ( ( 4, 4 ),
 ( 0.2699327958334041266, 1.570796326794896558 ),
 .UNSPECIFIED. ) 
 CURVE ( )  GEOMETRIC_REPRESENTATION_ITEM ( )  RATIONAL_B_SPLINE_CURVE ( ( 1.000000000000000000, 0.8638816171694810864, 0.8638816171694810864, 1.000000000000000000 ) ) 
 REPRESENTATION_ITEM ( '' )  );
#7217 = DIRECTION ( 'NONE',  ( 0.000000000000000000, 0.000000000000000000, 1.000000000000000000 ) ) ;
#7218 = EDGE_CURVE ( 'NONE', #7888, #11196, #8720, .T. ) ;
#7219 = CONTEXT_DEPENDENT_SHAPE_REPRESENTATION ( #10795, #8931 ) ;
#7220 = CARTESIAN_POINT ( 'NONE',  ( 4.967390183827647299, 49.34301876381886132, 24.50161767623307441 ) ) ;
#7221 = CARTESIAN_POINT ( 'NONE',  ( 28.59999999999998721, 12.86707612778636012, 88.47553407664152303 ) ) ;
#7222 = CARTESIAN_POINT ( 'NONE',  ( 42.47500000054623115, 13.07298590277314432, 88.54243821818161564 ) ) ;
#7223 = VECTOR ( 'NONE', #5885, 1000.000000000000000 ) ;
#7224 = CARTESIAN_POINT ( 'NONE',  ( 27.07500000054622902, 26.19570976099943849, 86.29171490190961435 ) ) ;
#7225 = EDGE_CURVE ( 'NONE', #7703, #1347, #12345, .T. ) ;
#7226 = CARTESIAN_POINT ( 'NONE',  ( 10.00000000000000355, 20.00000000000000355, 83.29316153445363113 ) ) ;
#7227 = PLANE ( 'NONE',  #5545 ) ;
#7228 = CARTESIAN_POINT ( 'NONE',  ( 3.061616997868383043E-15, 139.9999999999999716, 25.00000000000000000 ) ) ;
#7229 = CARTESIAN_POINT ( 'NONE',  ( -28.50000000000001066, 69.50000000000000000, 146.8533255156881978 ) ) ;
#7230 = ORIENTED_EDGE ( 'NONE', *, *, #11727, .T. ) ;
#7231 = DIRECTION ( 'NONE',  ( 0.000000000000000000, 0.000000000000000000, -1.000000000000000000 ) ) ;
#7232 = DIRECTION ( 'NONE',  ( 0.000000000000000000, 0.000000000000000000, 1.000000000000000000 ) ) ;
#7233 = ORIENTED_EDGE ( 'NONE', *, *, #10024, .T. ) ;
#7234 = EDGE_CURVE ( 'NONE', #8699, #7136, #4725, .T. ) ;
#7235 = VECTOR ( 'NONE', #10894, 999.9999999999998863 ) ;
#7236 =( NAMED_UNIT ( * ) PLANE_ANGLE_UNIT ( ) SI_UNIT ( $, .RADIAN. ) );
#7237 = CARTESIAN_POINT ( 'NONE',  ( 33.17500000054621978, 26.19570976099943849, 86.29171490190961435 ) ) ;
#7238 = CARTESIAN_POINT ( 'NONE',  ( -28.50000000000001066, 84.49999999999998579, 146.8533255156881978 ) ) ;
#7239 = CARTESIAN_POINT ( 'NONE',  ( 45.17500000054622689, 26.92701409722686634, 88.54243821818162985 ) ) ;
#7240 = CARTESIAN_POINT ( 'NONE',  ( 31.07500000054622546, 24.28113015263587471, 84.90069139318163138 ) ) ;
#7241 = CARTESIAN_POINT ( 'NONE',  ( 35.99999999999999289, 20.00000000000000355, 98.29316153445363113 ) ) ;
#7242 = CIRCLE ( 'NONE', #1763, 5.000000000000001776 ) ;
#7243 = CARTESIAN_POINT ( 'NONE',  ( 43.57500000054623257, 24.28113015263587116, 96.68563167572563088 ) ) ;
#7244 = VERTEX_POINT ( 'NONE', #7522 ) ;
#7245 = CARTESIAN_POINT ( 'NONE',  ( 24.95000000109246585, 26.37988106264029398, 86.15790661882942914 ) ) ;
#7246 = CARTESIAN_POINT ( 'NONE',  ( 3.061617023331388775E-15, 45.00000000000000711, 25.00000000000000000 ) ) ;
#7247 = ORIENTED_EDGE ( 'NONE', *, *, #6077, .T. ) ;
#7248 = CARTESIAN_POINT ( 'NONE',  ( 27.49999999999999645, 20.00000000000000355, 189.0000000000000000 ) ) ;
#7249 = ORIENTED_EDGE ( 'NONE', *, *, #9929, .F. ) ;
#7250 = CARTESIAN_POINT ( 'NONE',  ( 27.49999999999999645, 20.00000000000000355, 187.9999999999999716 ) ) ;
#7251 = DIRECTION ( 'NONE',  ( -1.000000000000000000, 0.000000000000000000, 0.000000000000000000 ) ) ;
#7252 = CARTESIAN_POINT ( 'NONE',  ( 39.99999999999998579, 20.00000000000000355, 98.29316153445363113 ) ) ;
#7253 = CARTESIAN_POINT ( 'NONE',  ( 25.19999999999998508, 24.40838939219355197, 84.72553407664153724 ) ) ;
#7254 = CARTESIAN_POINT ( 'NONE',  ( 25.67500000054623044, 22.36655054427230027, 98.07665518445361386 ) ) ;
#7255 = CARTESIAN_POINT ( 'NONE',  ( 26.47500000054622404, 13.07298590277314432, 88.54243821818161564 ) ) ;
#7256 = LINE ( 'NONE', #6127, #292 ) ;
#7257 = CARTESIAN_POINT ( 'NONE',  ( -2.067585255946370548, 45.44456205236168245, 24.91481882275639848 ) ) ;
#7258 = VECTOR ( 'NONE', #759, 1000.000000000000000 ) ;
#7259 = VERTEX_POINT ( 'NONE', #7006 ) ;
#7260 = CARTESIAN_POINT ( 'NONE',  ( 46.35000000109247509, 13.62011893735971135, 86.15790661882942914 ) ) ;
#7261 = ORIENTED_EDGE ( 'NONE', *, *, #4557, .T. ) ;
#7262 = DIRECTION ( 'NONE',  ( -0.000000000000000000, -0.000000000000000000, 1.000000000000000000 ) ) ;
#7263 = AXIS2_PLACEMENT_3D ( 'NONE', #10749, #8852, #4030 ) ;
#7264 = ORIENTED_EDGE ( 'NONE', *, *, #5433, .T. ) ;
#7265 = EDGE_CURVE ( 'NONE', #8987, #7598, #6957, .T. ) ;
#7266 = DIRECTION ( 'NONE',  ( -1.000000000000000000, -0.000000000000000000, -0.000000000000000000 ) ) ;
#7267 = CARTESIAN_POINT ( 'NONE',  ( 9.983753628317437290, 19.33993981085001579, -22.91999041428549688 ) ) ;
#7268 = VECTOR ( 'NONE', #675, 1000.000000000000000 ) ;
#7269 = CARTESIAN_POINT ( 'NONE',  ( 20.67500000054622333, 17.63344945572770328, 83.50966788445364841 ) ) ;
#7270 = AXIS2_PLACEMENT_3D ( 'NONE', #2445, #1563, #9306 ) ;
#7271 = CARTESIAN_POINT ( 'NONE',  ( 5.000000000000000000, 50.00000000000000000, 24.49489742783178059 ) ) ;
#7272 = CARTESIAN_POINT ( 'NONE',  ( -9.106574839427329593, 15.85560948713796492, 23.28279145951148266 ) ) ;
#7273 = CARTESIAN_POINT ( 'NONE',  ( 32.99999999999998579, 20.00000000000000355, 83.29316153445364534 ) ) ;
#7274 = CARTESIAN_POINT ( 'NONE',  ( 42.59999999999998721, 12.86707612778636012, 88.47553407664152303 ) ) ;
#7275 = CARTESIAN_POINT ( 'NONE',  ( -111.8465843842649292, 77.00000000000000000, 146.8533255156881978 ) ) ;
#7276 = CARTESIAN_POINT ( 'NONE',  ( -6.999999999999999112, 55.00000000000000000, 124.8533255156881694 ) ) ;
#7277 = VECTOR ( 'NONE', #4120, 1000.000000000000114 ) ;
#7278 = CARTESIAN_POINT ( 'NONE',  ( -4.486434092443181143, 52.21331568334087336, 24.59426911350885092 ) ) ;
#7279 = ORIENTED_EDGE ( 'NONE', *, *, #4557, .F. ) ;
#7280 = VECTOR ( 'NONE', #9989, 1000.000000000000000 ) ;
#7281 = CONTEXT_DEPENDENT_SHAPE_REPRESENTATION ( #11285, #3155 ) ;
#7282 = DIRECTION ( 'NONE',  ( -1.000000000000000000, -0.000000000000000000, -0.000000000000000000 ) ) ;
#7283 = ADVANCED_FACE ( 'NONE', ( #8909 ), #228, .F. ) ;
#7284 = CARTESIAN_POINT ( 'NONE',  ( 1.295572856795887295, 54.84026084924703071, 24.96846459459551681 ) ) ;
#7285 = CARTESIAN_POINT ( 'NONE',  ( 43.97500000054622404, 17.63344945572769973, 98.07665518445361386 ) ) ;
#7286 = CARTESIAN_POINT ( 'NONE',  ( 28.87500000054622262, 22.36655054427230382, 83.50966788445364841 ) ) ;
#7287 = LINE ( 'NONE', #11283, #4233 ) ;
#7288 = LINE ( 'NONE', #11158, #5628 ) ;
#7289 = CARTESIAN_POINT ( 'NONE',  ( 33.29999999999999005, 26.37988106264029398, 86.15790661882942914 ) ) ;
#7290 = FACE_OUTER_BOUND ( 'NONE', #7845, .T. ) ;
#7291 = ORIENTED_EDGE ( 'NONE', *, *, #7068, .T. ) ;
#7292 = CARTESIAN_POINT ( 'NONE',  ( 23.45000000109246585, 24.40838939219354842, 96.86078899226572503 ) ) ;
#7293 = ORIENTED_EDGE ( 'NONE', *, *, #7210, .T. ) ;
#7294 =( GEOMETRIC_REPRESENTATION_CONTEXT ( 3 ) GLOBAL_UNCERTAINTY_ASSIGNED_CONTEXT ( ( #4803 ) ) GLOBAL_UNIT_ASSIGNED_CONTEXT ( ( #4718, #10299, #666 ) ) REPRESENTATION_CONTEXT ( 'NONE', 'WORKASPACE' ) );
#7295 = CARTESIAN_POINT ( 'NONE',  ( 38.99999999999998579, 20.00000000000000355, 83.29316153445364534 ) ) ;
#7296 = ORIENTED_EDGE ( 'NONE', *, *, #7312, .T. ) ;
#7297 = CARTESIAN_POINT ( 'NONE',  ( 32.77500000054622831, 17.63344945572770328, 83.50966788445364841 ) ) ;
#7298 = DIRECTION ( 'NONE',  ( -1.000000000000000000, 0.000000000000000000, 0.000000000000000000 ) ) ;
#7299 = CARTESIAN_POINT ( 'NONE',  ( 43.77500000054622831, 20.00000000000000355, 98.07665518445361386 ) ) ;
#7300 = CARTESIAN_POINT ( 'NONE',  ( 32.07500000054622546, 15.71886984736413417, 96.68563167572563088 ) ) ;
#7301 = CARTESIAN_POINT ( 'NONE',  ( 34.69999999999998863, 13.62011893735971135, 86.15790661882942914 ) ) ;
#7302 = CIRCLE ( 'NONE', #4471, 5.035999999999999588 ) ;
#7303 = ADVANCED_FACE ( 'NONE', ( #1056 ), #9199, .F. ) ;
#7304 = CARTESIAN_POINT ( 'NONE',  ( 23.10660171779821681, 12.50000000000000711, 140.6066017177981848 ) ) ;
#7305 = CARTESIAN_POINT ( 'NONE',  ( 47.37500000054622973, 26.92701409722686634, 93.04388485072563242 ) ) ;
#7306 = ORIENTED_EDGE ( 'NONE', *, *, #7346, .F. ) ;
#7307 = CARTESIAN_POINT ( 'NONE',  ( 22.45000000109246585, 15.59161060780646046, 84.72553407664153724 ) ) ;
#7308 = CARTESIAN_POINT ( 'NONE',  ( 12.59999999999999964, 8.082668874372534964E-16, 6.600000000000003197 ) ) ;
#7309 = ORIENTED_EDGE ( 'NONE', *, *, #10691, .T. ) ;
#7310 = CARTESIAN_POINT ( 'NONE',  ( -0.3292543530451116363, 30.00000000000001421, 28.00000000000000355 ) ) ;
#7311 = EDGE_LOOP ( 'NONE', ( #7813, #2991, #11446, #9692, #895 ) ) ;
#7312 = EDGE_CURVE ( 'NONE', #10865, #136, #3008, .T. ) ;
#7313 = DIRECTION ( 'NONE',  ( 1.000000000000000000, 0.000000000000000000, -0.000000000000000000 ) ) ;
#7314 = VECTOR ( 'NONE', #4127, 1000.000000000000000 ) ;
#7315 = CYLINDRICAL_SURFACE ( 'NONE', #8905, 7.500000000000000000 ) ;
#7316 = DIRECTION ( 'NONE',  ( 0.000000000000000000, 0.000000000000000000, -1.000000000000000000 ) ) ;
#7317 = CARTESIAN_POINT ( 'NONE',  ( 121.9999999999999858, 6.757601037695095565E-16, -5.035999999999999588 ) ) ;
#7318 = CARTESIAN_POINT ( 'NONE',  ( 22.87500000054623328, 22.36655054427230382, 83.50966788445364841 ) ) ;
#7319 = CARTESIAN_POINT ( 'NONE',  ( 23.17500000054622689, 26.19570976099943493, 86.29171490190961435 ) ) ;
#7320 = DIRECTION ( 'NONE',  ( 0.000000000000000000, 0.000000000000000000, 1.000000000000000000 ) ) ;
#7321 = DIRECTION ( 'NONE',  ( 0.000000000000000000, -0.5000000000000009992, -0.8660254037844380415 ) ) ;
#7322 = ORIENTED_EDGE ( 'NONE', *, *, #5608, .T. ) ;
#7323 = CARTESIAN_POINT ( 'NONE',  ( 41.85000000109246798, 15.59161060780645691, 96.86078899226572503 ) ) ;
#7324 = CARTESIAN_POINT ( 'NONE',  ( 3.968701803879573831, 53.04568146648268367, -24.68320166897649770 ) ) ;
#7325 = VERTEX_POINT ( 'NONE', #9868 ) ;
#7326 = CARTESIAN_POINT ( 'NONE',  ( 4.999999999999999112, 0.000000000000000000, 121.2488769092545198 ) ) ;
#7327 = ORIENTED_EDGE ( 'NONE', *, *, #5126, .T. ) ;
#7328 = CARTESIAN_POINT ( 'NONE',  ( -0.3289793214801078336, 10.00000000000000000, -25.00000000000000355 ) ) ;
#7329 = CARTESIAN_POINT ( 'NONE',  ( 8.653999659896598473, 14.97853430653165319, -23.45497003317995421 ) ) ;
#7330 = CARTESIAN_POINT ( 'NONE',  ( 20.77500000054622831, 20.00000000000000355, 83.50966788445364841 ) ) ;
#7331 = DIRECTION ( 'NONE',  ( -0.000000000000000000, 0.000000000000000000, 1.000000000000000000 ) ) ;
#7332 = CARTESIAN_POINT ( 'NONE',  ( -6.851336394414588860, 12.70864359358585460, 24.04404201862471524 ) ) ;
#7333 = ADVANCED_FACE ( 'NONE', ( #7960 ), #8388, .T. ) ;
#7334 = FACE_OUTER_BOUND ( 'NONE', #4805, .T. ) ;
#7335 =( BOUNDED_CURVE ( )  B_SPLINE_CURVE ( 3, ( #241, #2203, #5061, #9165 ),
 .UNSPECIFIED., .F., .F. ) 
 B_SPLINE_CURVE_WITH_KNOTS ( ( 4, 4 ),
 ( 1.570796326794896558, 2.871659857756389211 ),
 .UNSPECIFIED. ) 
 CURVE ( )  GEOMETRIC_REPRESENTATION_ITEM ( )  RATIONAL_B_SPLINE_CURVE ( ( 1.000000000000000000, 0.8638816171694809753, 0.8638816171694809753, 1.000000000000000000 ) ) 
 REPRESENTATION_ITEM ( '' )  );
#7336 = CARTESIAN_POINT ( 'NONE',  ( -1.659969451079500224, 10.13322420983673311, 20.93680794575981352 ) ) ;
#7337 = FACE_OUTER_BOUND ( 'NONE', #1982, .T. ) ;
#7338 = CARTESIAN_POINT ( 'NONE',  ( 5.000000000000000000, 50.00000000000000000, 24.49489742783178059 ) ) ;
#7339 = CARTESIAN_POINT ( 'NONE',  ( 23.49999999999998579, 27.88596668178699645, 90.79316153445363113 ) ) ;
#7340 = ORIENTED_EDGE ( 'NONE', *, *, #3179, .F. ) ;
#7341 = EDGE_CURVE ( 'NONE', #2752, #6613, #2186, .T. ) ;
#7342 = CARTESIAN_POINT ( 'NONE',  ( 5.000000000000000000, 50.00000000000000000, 24.49489742783178059 ) ) ;
#7343 = CARTESIAN_POINT ( 'NONE',  ( 28.09999999999999076, 17.56310227825320425, 98.29316153445363113 ) ) ;
#7344 = CARTESIAN_POINT ( 'NONE',  ( 40.47500000054622404, 13.07298590277314432, 88.54243821818161564 ) ) ;
#7345 = CARTESIAN_POINT ( 'NONE',  ( 29.77500000054622831, 20.00000000000000355, 98.07665518445361386 ) ) ;
#7346 = EDGE_CURVE ( 'NONE', #3859, #6557, #8841, .T. ) ;
#7347 = CARTESIAN_POINT ( 'NONE',  ( 6.909847264846026071, 12.77053099975849548, 92.80456193764219108 ) ) ;
#7348 = DIRECTION ( 'NONE',  ( -1.000000000000000000, -0.000000000000000000, -0.000000000000000000 ) ) ;
#7349 = VECTOR ( 'NONE', #2539, 1000.000000000000114 ) ;
#7350 = CARTESIAN_POINT ( 'NONE',  ( 35.19999999999998863, 24.40838939219355197, 84.72553407664153724 ) ) ;
#7351 = CARTESIAN_POINT ( 'NONE',  ( 31.29999999999998650, 26.37988106264029398, 86.15790661882942914 ) ) ;
#7352 = ORIENTED_EDGE ( 'NONE', *, *, #28, .T. ) ;
#7353 = ADVANCED_FACE ( 'NONE', ( #3072 ), #2313, .T. ) ;
#7354 = CARTESIAN_POINT ( 'NONE',  ( 6.000000000000000000, -5.839897972853063557, 6.938893903907228378E-15 ) ) ;
#7355 = ORIENTED_EDGE ( 'NONE', *, *, #10906, .F. ) ;
#7356 = DIRECTION ( 'NONE',  ( 1.000000000000000000, 0.000000000000000000, 0.000000000000000000 ) ) ;
#7357 = CARTESIAN_POINT ( 'NONE',  ( -70.39081644922404735, 20.00000000000000355, 145.0000000000000568 ) ) ;
#7358 = PRODUCT_RELATED_PRODUCT_CATEGORY ( 'part', '', ( #5993 ) ) ;
#7359 = EDGE_CURVE ( 'NONE', #2741, #5525, #1240, .T. ) ;
#7360 = CARTESIAN_POINT ( 'NONE',  ( 30.37500000054622618, 12.34168156654572357, 90.79316153445363113 ) ) ;
#7361 = CARTESIAN_POINT ( 'NONE',  ( -2.508609049021579551, 54.33766627009165262, -27.88875238525115208 ) ) ;
#7362 = CARTESIAN_POINT ( 'NONE',  ( 43.07500000054622546, 26.19570976099943849, 86.29171490190961435 ) ) ;
#7363 = CARTESIAN_POINT ( 'NONE',  ( 35.27500000054622120, 26.92701409722686634, 88.54243821818162985 ) ) ;
#7364 = CARTESIAN_POINT ( 'NONE',  ( 32.99999999999998579, 20.00000000000000355, 83.29316153445364534 ) ) ;
#7365 = CARTESIAN_POINT ( 'NONE',  ( 27.50000000000000355, 12.50000000000001066, 145.0000000000000000 ) ) ;
#7366 = CARTESIAN_POINT ( 'NONE',  ( 40.97500000054622404, 24.28113015263587471, 84.90069139318163138 ) ) ;
#7367 = EDGE_LOOP ( 'NONE', ( #4734, #2115, #5165, #8410, #6857 ) ) ;
#7368 = CIRCLE ( 'NONE', #11630, 5.057500000000000107 ) ;
#7369 = CARTESIAN_POINT ( 'NONE',  ( 48.07500000054623257, 13.80429023900056507, 95.29460816699764791 ) ) ;
#7370 = CARTESIAN_POINT ( 'NONE',  ( -3.765972656198162571, 46.69472370319601850, -20.66089928520440111 ) ) ;
#7371 = EDGE_LOOP ( 'NONE', ( #11887, #3794, #1132, #11904 ) ) ;
#7372 = VECTOR ( 'NONE', #5269, 1000.000000000000000 ) ;
#7373 = CARTESIAN_POINT ( 'NONE',  ( 0.000000000000000000, 139.9999999999999716, 0.000000000000000000 ) ) ;
#7374 = ORIENTED_EDGE ( 'NONE', *, *, #5526, .T. ) ;
#7375 = CARTESIAN_POINT ( 'NONE',  ( 0.000000000000000000, 0.000000000000000000, 6.500000000000000888 ) ) ;
#7376 = EDGE_CURVE ( 'NONE', #9352, #12263, #5996, .T. ) ;
#7377 = CARTESIAN_POINT ( 'NONE',  ( -23.99529484836403981, 12.50000000000001243, 148.5047051516359602 ) ) ;
#7378 = CARTESIAN_POINT ( 'NONE',  ( 32.15000000109246514, 12.11403331821300533, 90.79316153445363113 ) ) ;
#7379 = CARTESIAN_POINT ( 'NONE',  ( 27.27500000054622475, 27.65831843345427998, 90.79316153445363113 ) ) ;
#7380 = CARTESIAN_POINT ( 'NONE',  ( 21.97500000054622049, 17.63344945572769973, 98.07665518445361386 ) ) ;
#7381 = VECTOR ( 'NONE', #5695, 1000.000000000000000 ) ;
#7382 = DIRECTION ( 'NONE',  ( 0.000000000000000000, 0.000000000000000000, 1.000000000000000000 ) ) ;
#7383 = EDGE_CURVE ( 'NONE', #10526, #10, #9741, .T. ) ;
#7384 = CARTESIAN_POINT ( 'NONE',  ( 39.25000000109246656, 27.13292387221364876, 93.11078899226573924 ) ) ;
#7385 = ORIENTED_EDGE ( 'NONE', *, *, #11576, .F. ) ;
#7386 = CARTESIAN_POINT ( 'NONE',  ( 41.35000000109245377, 26.37988106264029398, 95.42841645007781892 ) ) ;
#7387 = CARTESIAN_POINT ( 'NONE',  ( 3.761098173404043621, 53.29862245996868353, -24.71568690466639140 ) ) ;
#7388 = ORIENTED_EDGE ( 'NONE', *, *, #3871, .T. ) ;
#7389 = LINE ( 'NONE', #6379, #1605 ) ;
#7390 = ORIENTED_EDGE ( 'NONE', *, *, #3016, .T. ) ;
#7391 = CARTESIAN_POINT ( 'NONE',  ( -6.110563603929655585, 12.05744620208248286, -24.24805373538051967 ) ) ;
#7392 = LINE ( 'NONE', #5248, #1180 ) ;
#7393 =( REPRESENTATION_RELATIONSHIP ('NONE','NONE', #4262, #7408 ) REPRESENTATION_RELATIONSHIP_WITH_TRANSFORMATION ( #11673 )SHAPE_REPRESENTATION_RELATIONSHIP( ) );
#7394 = CARTESIAN_POINT ( 'NONE',  ( 29.39999999999998792, 27.13292387221364876, 88.47553407664153724 ) ) ;
#7395 = CARTESIAN_POINT ( 'NONE',  ( 13.64110105645934290, 20.00000000000000355, 162.0000000000000000 ) ) ;
#7396 = DIRECTION ( 'NONE',  ( 0.000000000000000000, 0.000000000000000000, 1.000000000000000000 ) ) ;
#7397 = CARTESIAN_POINT ( 'NONE',  ( 10.00000000000000355, 20.00000000000000355, 18.46618531261938401 ) ) ;
#7398 = AXIS2_PLACEMENT_3D ( 'NONE', #7460, #10558, #2639 ) ;
#7399 = CARTESIAN_POINT ( 'NONE',  ( -8.656678912164643691, 14.98331879925162902, 19.13349105540200057 ) ) ;
#7400 = DIRECTION ( 'NONE',  ( 0.000000000000000000, 0.000000000000000000, -1.000000000000000000 ) ) ;
#7401 = CARTESIAN_POINT ( 'NONE',  ( 26.57500000054622902, 15.71886984736413773, 84.90069139318163138 ) ) ;
#7402 = CARTESIAN_POINT ( 'NONE',  ( 26.99999999999998934, 20.00000000000000355, 83.29316153445364534 ) ) ;
#7403 = PLANE ( 'NONE',  #5499 ) ;
#7404 = ORIENTED_EDGE ( 'NONE', *, *, #2428, .F. ) ;
#7405 = AXIS2_PLACEMENT_3D ( 'NONE', #8112, #1140, #2213 ) ;
#7406 = FACE_OUTER_BOUND ( 'NONE', #9610, .T. ) ;
#7407 = VECTOR ( 'NONE', #2200, 1000.000000000000000 ) ;
#7408 = SHAPE_REPRESENTATION ( 'Cast Iron Bearing Support Block', ( #9021 ), #309 ) ;
#7409 = CARTESIAN_POINT ( 'NONE',  ( 4.337826254667723092, 52.50833866356535395, 24.62149076657007640 ) ) ;
#7410 = CARTESIAN_POINT ( 'NONE',  ( 36.37500000054622973, 13.07298590277314432, 88.54243821818161564 ) ) ;
#7411 = CARTESIAN_POINT ( 'NONE',  ( 37.37500000054622262, 27.65831843345427998, 90.79316153445363113 ) ) ;
#7412 = CARTESIAN_POINT ( 'NONE',  ( 28.97500000054622760, 24.28113015263587471, 84.90069139318163138 ) ) ;
#7413 = CARTESIAN_POINT ( 'NONE',  ( 6.909788229321696562, 12.77047530449378776, 88.78197206557399568 ) ) ;
#7414 = CARTESIAN_POINT ( 'NONE',  ( 2.505975641493357831, 45.66085398937747186, 24.87560495202607669 ) ) ;
#7415 = AXIS2_PLACEMENT_3D ( 'NONE', #4199, #11940, #10924 ) ;
#7416 = CYLINDRICAL_SURFACE ( 'NONE', #3521, 7.499999999999992895 ) ;
#7417 = DIRECTION ( 'NONE',  ( 0.000000000000000000, -1.000000000000000000, 1.039664082171044875E-15 ) ) ;
#7418 = VERTEX_POINT ( 'NONE', #7064 ) ;
#7419 = CARTESIAN_POINT ( 'NONE',  ( 9.739739614376460963, 17.70973893131317922, 23.02482158226496622 ) ) ;
#7420 = ORIENTED_EDGE ( 'NONE', *, *, #456, .T. ) ;
#7421 = CARTESIAN_POINT ( 'NONE',  ( 12.00000000000000355, 0.000000000000000000, 9.000000000000000000 ) ) ;
#7422 = EDGE_CURVE ( 'NONE', #11877, #110, #734, .T. ) ;
#7423 = DIRECTION ( 'NONE',  ( -0.9499795115074031182, 0.3123122279324910822, 0.000000000000000000 ) ) ;
#7424 = AXIS2_PLACEMENT_3D ( 'NONE', #11211, #10146, #1457 ) ;
#7425 = CARTESIAN_POINT ( 'NONE',  ( 32.17500000054622689, 13.80429023900056507, 95.29460816699764791 ) ) ;
#7426 = DIRECTION ( 'NONE',  ( -1.000000000000000000, -0.000000000000000000, -0.000000000000000000 ) ) ;
#7427 = CARTESIAN_POINT ( 'NONE',  ( 46.77500000054622831, 20.00000000000000355, 83.50966788445364841 ) ) ;
#7428 = CARTESIAN_POINT ( 'NONE',  ( 35.97500000054620983, 17.63344945572769973, 98.07665518445361386 ) ) ;
#7429 = CARTESIAN_POINT ( 'NONE',  ( 27.49999999999998934, 27.88596668178699645, 90.79316153445363113 ) ) ;
#7430 = CARTESIAN_POINT ( 'NONE',  ( 20.00000000000001066, 15.60660171779821681, 137.4999999999999716 ) ) ;
#7431 = CARTESIAN_POINT ( 'NONE',  ( 37.57500000054622546, 24.28113015263587116, 96.68563167572563088 ) ) ;
#7432 = EDGE_LOOP ( 'NONE', ( #11936, #3825 ) ) ;
#7433 = CARTESIAN_POINT ( 'NONE',  ( 21.65000000109246514, 20.00000000000000355, 98.29316153445363113 ) ) ;
#7434 = CARTESIAN_POINT ( 'NONE',  ( 6.000000000000000000, 0.000000000000000000, 0.000000000000000000 ) ) ;
#7435 = PRESENTATION_LAYER_ASSIGNMENT (  '', '', ( #9065 ) ) ;
#7436 = EDGE_LOOP ( 'NONE', ( #8729, #10872, #5100, #8405 ) ) ;
#7437 = CARTESIAN_POINT ( 'NONE',  ( 0.6651180000198534392, 9.999999999999987566, 21.00000000000000000 ) ) ;
#7438 = ORIENTED_EDGE ( 'NONE', *, *, #3535, .F. ) ;
#7439 = CARTESIAN_POINT ( 'NONE',  ( 10.00000000000000355, 20.00000000000000355, -22.91287847477919826 ) ) ;
#7440 = DIRECTION ( 'NONE',  ( -0.000000000000000000, -0.000000000000000000, -1.000000000000000000 ) ) ;
#7441 = CARTESIAN_POINT ( 'NONE',  ( 3.302118497427160904, 46.23115272073012960, -27.80559317508241790 ) ) ;
#7442 = CARTESIAN_POINT ( 'NONE',  ( -34.72841614740048044, 22.00000000000000000, 170.0000119999999697 ) ) ;
#7443 = EDGE_CURVE ( 'NONE', #8699, #6932, #6935, .T. ) ;
#7444 = AXIS2_PLACEMENT_3D ( 'NONE', #5745, #9614, #4538 ) ;
#7445 = CARTESIAN_POINT ( 'NONE',  ( 22.47500000054623115, 13.80429023900056684, 86.29171490190961435 ) ) ;
#7446 = CARTESIAN_POINT ( 'NONE',  ( 23.07500000054622546, 24.28113015263587471, 84.90069139318163138 ) ) ;
#7447 = DIRECTION ( 'NONE',  ( 0.000000000000000000, -0.5000000000000011102, -0.8660254037844379305 ) ) ;
#7448 = PLANE ( 'NONE',  #6248 ) ;
#7449 = ORIENTED_EDGE ( 'NONE', *, *, #4123, .T. ) ;
#7450 = CARTESIAN_POINT ( 'NONE',  ( 35.65000000109246514, 20.00000000000000355, 98.29316153445363113 ) ) ;
#7451 = CARTESIAN_POINT ( 'NONE',  ( 3.055841136373902422, 53.97118948954670969, -24.81406232681816348 ) ) ;
#7452 = VERTEX_POINT ( 'NONE', #9804 ) ;
#7453 = CARTESIAN_POINT ( 'NONE',  ( 29.95000000109246230, 13.62011893735970958, 95.42841645007781892 ) ) ;
#7454 = EDGE_LOOP ( 'NONE', ( #1720, #1984, #8524, #11760 ) ) ;
#7455 = CARTESIAN_POINT ( 'NONE',  ( 47.99999999999998579, 20.00000000000000355, 98.29316153445363113 ) ) ;
#7456 = CARTESIAN_POINT ( 'NONE',  ( 5.041410851502566182, 11.35764812998954731, -20.38800383682523076 ) ) ;
#7457 = EDGE_CURVE ( 'NONE', #409, #7687, #12041, .T. ) ;
#7458 = CARTESIAN_POINT ( 'NONE',  ( 29.59999999999998721, 27.13292387221364876, 93.11078899226573924 ) ) ;
#7459 = AXIS2_PLACEMENT_3D ( 'NONE', #6819, #2057, #4027 ) ;
#7460 = CARTESIAN_POINT ( 'NONE',  ( 6.000000000000000000, 8.759846959279592227, -5.057500000000009877 ) ) ;
#7461 = CARTESIAN_POINT ( 'NONE',  ( 27.99999999999998579, 20.00000000000000355, 98.29316153445363113 ) ) ;
#7462 = CARTESIAN_POINT ( 'NONE',  ( 1.766167014948355707, 54.68054567383913422, -27.94465362560199040 ) ) ;
#7463 = EDGE_CURVE ( 'NONE', #10754, #8571, #7896, .T. ) ;
#7464 = DIRECTION ( 'NONE',  ( 0.000000000000000000, 0.000000000000000000, -1.000000000000000000 ) ) ;
#7465 = CARTESIAN_POINT ( 'NONE',  ( 47.77500000054622120, 22.36655054427230027, 98.07665518445361386 ) ) ;
#7466 = LINE ( 'NONE', #1452, #12277 ) ;
#7467 = DIRECTION ( 'NONE',  ( 0.000000000000000000, -0.4999999999999987232, 0.8660254037844392627 ) ) ;
#7468 = EDGE_LOOP ( 'NONE', ( #1479, #7390, #11601, #9814 ) ) ;
#7469 = VECTOR ( 'NONE', #2656, 1000.000000000000000 ) ;
#7470 = EDGE_CURVE ( 'NONE', #5467, #5847, #10177, .T. ) ;
#7471 = CARTESIAN_POINT ( 'NONE',  ( 4.999999999999999112, 18.00000000000000355, 169.9999999999999716 ) ) ;
#7472 = DIRECTION ( 'NONE',  ( -1.224646799147353207E-16, 1.000000000000000000, 0.000000000000000000 ) ) ;
#7473 = CARTESIAN_POINT ( 'NONE',  ( 39.57500000054622546, 24.28113015263587116, 96.68563167572563088 ) ) ;
#7474 = CARTESIAN_POINT ( 'NONE',  ( 35.37500000054622973, 27.65831843345427998, 90.79316153445363113 ) ) ;
#7475 = DIRECTION ( 'NONE',  ( 0.000000000000000000, -0.5000000000000012212, -0.8660254037844380415 ) ) ;
#7476 = VECTOR ( 'NONE', #8598, 1000.000000000000000 ) ;
#7477 = DIRECTION ( 'NONE',  ( 1.000000000000000000, 0.000000000000000000, 0.000000000000000000 ) ) ;
#7478 = CARTESIAN_POINT ( 'NONE',  ( -10.00000000000000178, 20.32878730486446273, 22.91287847477919826 ) ) ;
#7479 = FACE_OUTER_BOUND ( 'NONE', #9778, .T. ) ;
#7480 = CARTESIAN_POINT ( 'NONE',  ( -21.00000000000001776, 81.39339828220178674, 154.3533255156881694 ) ) ;
#7481 = CARTESIAN_POINT ( 'NONE',  ( 9.933637772289912959, 18.67556250305220189, 22.94215742280771408 ) ) ;
#7482 = ORIENTED_EDGE ( 'NONE', *, *, #4358, .F. ) ;
#7483 = ADVANCED_BREP_SHAPE_REPRESENTATION ( '', ( #6058, #9021 ), #309 ) ;
#7484 = EDGE_CURVE ( 'NONE', #9352, #6763, #9820, .T. ) ;
#7485 = FACE_OUTER_BOUND ( 'NONE', #420, .T. ) ;
#7486 = DIRECTION ( 'NONE',  ( 0.000000000000000000, 0.000000000000000000, 1.000000000000000000 ) ) ;
#7487 = CARTESIAN_POINT ( 'NONE',  ( 25.47500000054622404, 26.92701409722686634, 93.04388485072563242 ) ) ;
#7488 = CARTESIAN_POINT ( 'NONE',  ( 34.72841614740048044, 22.00000000000000000, 170.0000119999999697 ) ) ;
#7489 = CARTESIAN_POINT ( 'NONE',  ( 46.57500000054622546, 15.71886984736413773, 84.90069139318163138 ) ) ;
#7490 = CARTESIAN_POINT ( 'NONE',  ( 29.37500000054622618, 27.65831843345427998, 90.79316153445363113 ) ) ;
#7491 = CARTESIAN_POINT ( 'NONE',  ( 27.19999999999998863, 24.40838939219355197, 84.72553407664153724 ) ) ;
#7492 = CARTESIAN_POINT ( 'NONE',  ( 2.612127725832936065, 29.65839247515747346, 24.86517017815632968 ) ) ;
#7493 = EDGE_CURVE ( 'NONE', #10109, #6932, #7368, .T. ) ;
#7494 = CARTESIAN_POINT ( 'NONE',  ( 41.27500000054622831, 27.65831843345427998, 90.79316153445363113 ) ) ;
#7495 = EDGE_LOOP ( 'NONE', ( #8435, #9099 ) ) ;
#7496 = AXIS2_PLACEMENT_3D ( 'NONE', #12319, #202, #8633 ) ;
#7497 = CARTESIAN_POINT ( 'NONE',  ( 49.67500000054621978, 22.36655054427230027, 98.07665518445361386 ) ) ;
#7498 = CARTESIAN_POINT ( 'NONE',  ( -4.491762996560707322, 47.77920471472745589, -20.51440311031020158 ) ) ;
#7499 = ORIENTED_EDGE ( 'NONE', *, *, #3853, .F. ) ;
#7500 = CARTESIAN_POINT ( 'NONE',  ( -5.024113554834485740, 28.67061468857206563, -27.55106389568239322 ) ) ;
#7501 = ORIENTED_EDGE ( 'NONE', *, *, #1120, .T. ) ;
#7502 = CARTESIAN_POINT ( 'NONE',  ( 7.942143053965557975, 26.11098614794844863, -23.70800582113895061 ) ) ;
#7503 = CARTESIAN_POINT ( 'NONE',  ( 10.00000000000003020, 20.00000000000000711, 172.0000000000000000 ) ) ;
#7504 = FACE_OUTER_BOUND ( 'NONE', #6376, .T. ) ;
#7505 = VECTOR ( 'NONE', #10080, 1000.000000000000000 ) ;
#7506 = CARTESIAN_POINT ( 'NONE',  ( 30.99999999999998934, 20.00000000000000355, 83.29316153445364534 ) ) ;
#7507 = CARTESIAN_POINT ( 'NONE',  ( 26.87500000054622618, 22.36655054427230382, 83.50966788445364841 ) ) ;
#7508 = CARTESIAN_POINT ( 'NONE',  ( 49.59999999999999432, 27.13292387221364876, 93.11078899226573924 ) ) ;
#7509 = B_SPLINE_CURVE_WITH_KNOTS ( 'NONE', 3,
 ( #12245, #3546, #7481, #7419, #11354, #10640, #6774, #1018, #1142, #7860, #7735, #9703, #3858, #1824, #10702, #11600, #10514, #5006, #11789, #8743, #948, #9641, #6644, #5710 ),
 .UNSPECIFIED., .F., .F.,
 ( 4, 2, 2, 2, 2, 2, 2, 2, 2, 2, 2, 4 ),
 ( 0.000000000000000000, 0.001975470015275241145, 0.002963205022912861284, 0.003950940030550481423, 0.005926410045825732976, 0.006914145053463355284, 0.007901880061100976724, 0.009877350076376223073, 0.01185282009165146769, 0.01284055509928909086, 0.01382829010692671404, 0.01580376012220196039 ),
 .UNSPECIFIED. ) ;
#7510 = CARTESIAN_POINT ( 'NONE',  ( 40.99999999999998579, 20.00000000000000355, 83.29316153445364534 ) ) ;
#7511 = FACE_OUTER_BOUND ( 'NONE', #12060, .T. ) ;
#7512 = ORIENTED_EDGE ( 'NONE', *, *, #8600, .F. ) ;
#7513 = CARTESIAN_POINT ( 'NONE',  ( 37.55000000109247082, 22.43689772174679575, 98.29316153445363113 ) ) ;
#7514 = CARTESIAN_POINT ( 'NONE',  ( 3.307338549894080604, 53.76391169785250668, -24.78134996739077422 ) ) ;
#7515 = ORIENTED_EDGE ( 'NONE', *, *, #8294, .T. ) ;
#7516 = CARTESIAN_POINT ( 'NONE',  ( 6.000000000000000000, -2.919948986426523341, 5.057500000000002771 ) ) ;
#7517 = CIRCLE ( 'NONE', #2856, 5.057500000000000107 ) ;
#7518 = EDGE_CURVE ( 'NONE', #2354, #2307, #9293, .T. ) ;
#7519 = ORIENTED_EDGE ( 'NONE', *, *, #11659, .T. ) ;
#7520 = CARTESIAN_POINT ( 'NONE',  ( -9.673467176944807733, 17.38163042592174889, -23.05306748635229752 ) ) ;
#7521 = CARTESIAN_POINT ( 'NONE',  ( 4.468390986973521883, 11.04793033951060011, -20.52120868300845657 ) ) ;
#7522 = CARTESIAN_POINT ( 'NONE',  ( -6.999999999999999112, 69.50000000000000000, 101.8533255156881978 ) ) ;
#7523 = ADVANCED_FACE ( 'NONE', ( #11126 ), #2433, .F. ) ;
#7524 = CONICAL_SURFACE ( 'NONE', #2048, 5.057500000000000107, 1.047197551196592302 ) ;
#7525 = CARTESIAN_POINT ( 'NONE',  ( 41.35889894354065177, 20.00000000000000355, 187.9999999999999716 ) ) ;
#7526 = CARTESIAN_POINT ( 'NONE',  ( 19.99999999999999645, 20.00000000000000355, 188.9999999999999716 ) ) ;
#7527 = CARTESIAN_POINT ( 'NONE',  ( 4.743569837746959728, 51.61387508005228142, -27.59555274614490017 ) ) ;
#7528 = FACE_OUTER_BOUND ( 'NONE', #11539, .T. ) ;
#7529 = CARTESIAN_POINT ( 'NONE',  ( 20.27500000054623186, 12.34168156654572535, 90.79316153445363113 ) ) ;
#7530 = CARTESIAN_POINT ( 'NONE',  ( 46.35000000109246798, 13.62011893735970958, 86.15790661882942914 ) ) ;
#7531 = CARTESIAN_POINT ( 'NONE',  ( 47.45000000109246230, 24.40838939219354842, 96.86078899226572503 ) ) ;
#7532 = EDGE_LOOP ( 'NONE', ( #9427, #11342, #2407, #10425 ) ) ;
#7533 = VERTEX_POINT ( 'NONE', #5299 ) ;
#7534 = CARTESIAN_POINT ( 'NONE',  ( -9.739271384326251280, 22.29254948852628715, -18.60516067502140558 ) ) ;
#7535 = EDGE_CURVE ( 'NONE', #938, #10109, #8793, .T. ) ;
#7536 = PLANE ( 'NONE',  #3987 ) ;
#7537 = CARTESIAN_POINT ( 'NONE',  ( 37.77500000054622120, 22.36655054427230027, 98.07665518445361386 ) ) ;
#7538 = CARTESIAN_POINT ( 'NONE',  ( 20.57500000054622902, 15.71886984736413773, 84.90069139318163138 ) ) ;
#7539 = DIRECTION ( 'NONE',  ( 0.000000000000000000, 0.000000000000000000, -1.000000000000000000 ) ) ;
#7540 = CARTESIAN_POINT ( 'NONE',  ( 0.3271393060908659445, 45.00000000000000711, 25.00000000000000355 ) ) ;
#7541 = ADVANCED_FACE ( 'NONE', ( #8091 ), #2707, .T. ) ;
#7542 = CARTESIAN_POINT ( 'NONE',  ( 0.000000000000000000, 67.00000000000000000, 0.000000000000000000 ) ) ;
#7543 = DIRECTION ( 'NONE',  ( 1.000000000000000000, -0.000000000000000000, -0.000000000000000000 ) ) ;
#7544 = ADVANCED_FACE ( 'NONE', ( #3265 ), #9805, .T. ) ;
#7545 = FACE_OUTER_BOUND ( 'NONE', #5187, .T. ) ;
#7546 = VERTEX_POINT ( 'NONE', #7128 ) ;
#7547 = CARTESIAN_POINT ( 'NONE',  ( 3.061616997868383043E-15, 139.9999999999999716, 25.00000000000000000 ) ) ;
#7548 = SHAPE_DEFINITION_REPRESENTATION ( #8023, #4262 ) ;
#7549 =( BOUNDED_CURVE ( )  B_SPLINE_CURVE ( 2, ( #8700, #6915, #11, #5972, #4896, #10719, #8757, #2032, #1160, #5024, #11165 ),
 .UNSPECIFIED., .F., .F. ) 
 B_SPLINE_CURVE_WITH_KNOTS ( ( 3, 2, 2, 2, 2, 3 ),
 ( 0.000000000000000000, 0.006666666666666673166, 0.01333333333333334633, 0.02000000000000001429, 0.02666666666666669266, 0.03333333333333336063 ),
 .UNSPECIFIED. ) 
 CURVE ( )  GEOMETRIC_REPRESENTATION_ITEM ( )  RATIONAL_B_SPLINE_CURVE ( ( 1.000000000000000000, 0.9510565162951535312, 1.000000000000000000, 0.9510565162951535312, 1.000000000000000000, 0.9510565162951535312, 1.000000000000000000, 0.9510565162951535312, 1.000000000000000000, 0.9510565162951533091, 1.000000000000000222 ) ) 
 REPRESENTATION_ITEM ( '' )  );
#7550 = CARTESIAN_POINT ( 'NONE',  ( 26.57500000054622191, 13.80429023900056684, 86.29171490190961435 ) ) ;
#7551 = CARTESIAN_POINT ( 'NONE',  ( 29.15000000109246159, 27.88596668178699645, 90.79316153445363113 ) ) ;
#7552 = AXIS2_PLACEMENT_3D ( 'NONE', #4004, #3059, #2038 ) ;
#7553 = CARTESIAN_POINT ( 'NONE',  ( 39.67500000054623399, 22.36655054427230027, 98.07665518445361386 ) ) ;
#7554 = CARTESIAN_POINT ( 'NONE',  ( 25.77500000054622831, 22.36655054427230027, 98.07665518445361386 ) ) ;
#7555 = CARTESIAN_POINT ( 'NONE',  ( 31.99999999999998579, 20.00000000000000355, 98.29316153445363113 ) ) ;
#7556 = SURFACE_STYLE_FILL_AREA ( #4829 ) ;
#7557 = CARTESIAN_POINT ( 'NONE',  ( 36.77500000054622831, 20.00000000000000355, 83.50966788445364841 ) ) ;
#7558 = ORIENTED_EDGE ( 'NONE', *, *, #12046, .T. ) ;
#7559 = CARTESIAN_POINT ( 'NONE',  ( 46.97500000054623115, 24.28113015263587471, 84.90069139318163138 ) ) ;
#7560 = CARTESIAN_POINT ( 'NONE',  ( 28.55000000109246372, 17.56310227825320425, 83.29316153445363113 ) ) ;
#7561 = EDGE_LOOP ( 'NONE', ( #7625, #7788 ) ) ;
#7562 = APPLICATION_CONTEXT ( 'automotive_design' ) ;
#7563 = CARTESIAN_POINT ( 'NONE',  ( 6.106435932944510370, 12.07435209537243814, 20.09427717736598851 ) ) ;
#7564 = VERTEX_POINT ( 'NONE', #6183 ) ;
#7565 = AXIS2_PLACEMENT_3D ( 'NONE', #499, #2577, #12105 ) ;
#7566 = CARTESIAN_POINT ( 'NONE',  ( 1.326742001580319741, 29.91711497655587948, -24.96694321103489855 ) ) ;
#7567 = DIRECTION ( 'NONE',  ( 0.000000000000000000, 0.000000000000000000, -1.000000000000000000 ) ) ;
#7568 = CARTESIAN_POINT ( 'NONE',  ( 44.27500000054622120, 13.07298590277314254, 93.04388485072563242 ) ) ;
#7569 = LINE ( 'NONE', #1909, #6760 ) ;
#7570 = CARTESIAN_POINT ( 'NONE',  ( 43.27500000054622120, 26.92701409722686634, 88.54243821818162985 ) ) ;
#7571 = CARTESIAN_POINT ( 'NONE',  ( 49.09999999999999432, 22.43689772174679575, 83.29316153445363113 ) ) ;
#7572 = VECTOR ( 'NONE', #6748, 1000.000000000000000 ) ;
#7573 = CARTESIAN_POINT ( 'NONE',  ( 41.49999999999997158, 27.88596668178699645, 90.79316153445363113 ) ) ;
#7574 = FACE_OUTER_BOUND ( 'NONE', #7432, .T. ) ;
#7575 = ORIENTED_EDGE ( 'NONE', *, *, #3789, .F. ) ;
#7576 = CARTESIAN_POINT ( 'NONE',  ( 6.000000000000000000, 0.000000000000000000, 0.000000000000000000 ) ) ;
#7577 = CARTESIAN_POINT ( 'NONE',  ( 40.25000000109246656, 12.86707612778636012, 88.47553407664152303 ) ) ;
#7578 = CARTESIAN_POINT ( 'NONE',  ( 6.612460753110299017, 12.47060822435505756, 24.11434807139940517 ) ) ;
#7579 = ORIENTED_EDGE ( 'NONE', *, *, #10397, .F. ) ;
#7580 = DIRECTION ( 'NONE',  ( 1.000000000000000000, 0.000000000000000000, 0.000000000000000000 ) ) ;
#7581 = ORIENTED_EDGE ( 'NONE', *, *, #854, .F. ) ;
#7582 = DIRECTION ( 'NONE',  ( 0.000000000000000000, 0.000000000000000000, -1.000000000000000000 ) ) ;
#7583 = VECTOR ( 'NONE', #1849, 1000.000000000000000 ) ;
#7584 = CARTESIAN_POINT ( 'NONE',  ( 30.75000000109246301, 22.43689772174679575, 83.29316153445363113 ) ) ;
#7585 = ADVANCED_FACE ( 'NONE', ( #3453 ), #10120, .T. ) ;
#7586 = CIRCLE ( 'NONE', #1893, 7.500000000000000000 ) ;
#7587 = CARTESIAN_POINT ( 'NONE',  ( -9.481431770954213079, 23.24517152888003224, 23.13387126485941536 ) ) ;
#7588 = FACE_OUTER_BOUND ( 'NONE', #8796, .T. ) ;
#7589 = CARTESIAN_POINT ( 'NONE',  ( 27.59999999999999076, 27.13292387221364876, 93.11078899226573924 ) ) ;
#7590 = VERTEX_POINT ( 'NONE', #7317 ) ;
#7591 = CARTESIAN_POINT ( 'NONE',  ( 6.000000000000000000, -2.919948986426525117, 5.057500000000004547 ) ) ;
#7592 = CARTESIAN_POINT ( 'NONE',  ( -50.00000000000001421, 55.00000000000000000, 124.8533255156881694 ) ) ;
#7593 = CARTESIAN_POINT ( 'NONE',  ( 20.07500000054622546, 13.80429023900056507, 95.29460816699764791 ) ) ;
#7594 = CARTESIAN_POINT ( 'NONE',  ( 46.55000000109247793, 17.56310227825318648, 83.29316153445365956 ) ) ;
#7595 = CIRCLE ( 'NONE', #4354, 7.499999999999978684 ) ;
#7596 = FACE_OUTER_BOUND ( 'NONE', #6559, .T. ) ;
#7597 = ORIENTED_EDGE ( 'NONE', *, *, #4345, .T. ) ;
#7598 = VERTEX_POINT ( 'NONE', #10058 ) ;
#7599 = CARTESIAN_POINT ( 'NONE',  ( -5.045054645757931944, 28.65860100811472932, -20.39267833245444805 ) ) ;
#7600 = CARTESIAN_POINT ( 'NONE',  ( 0.000000000000000000, 2.919948986426526005, -5.057500000000003659 ) ) ;
#7601 = AXIS2_PLACEMENT_3D ( 'NONE', #7395, #10541, #2933 ) ;
#7602 = EDGE_CURVE ( 'NONE', #5150, #1332, #5235, .T. ) ;
#7603 = EDGE_CURVE ( 'NONE', #1411, #5847, #7704, .T. ) ;
#7604 = LINE ( 'NONE', #7730, #4163 ) ;
#7605 = CARTESIAN_POINT ( 'NONE',  ( 6.000000000000000000, 5.839897972853065333, -6.938893903907228378E-15 ) ) ;
#7606 = CYLINDRICAL_SURFACE ( 'NONE', #5571, 10.00000000000000355 ) ;
#7607 = DIRECTION ( 'NONE',  ( 1.000000000000000000, -0.000000000000000000, -0.000000000000000000 ) ) ;
#7608 = CARTESIAN_POINT ( 'NONE',  ( 10.00000000000000355, 20.00000000000000355, -18.46618531261938401 ) ) ;
#7609 = EDGE_CURVE ( 'NONE', #438, #1603, #11418, .T. ) ;
#7610 = CYLINDRICAL_SURFACE ( 'NONE', #6297, 7.499999999999992895 ) ;
#7611 = ORIENTED_EDGE ( 'NONE', *, *, #6150, .F. ) ;
#7612 = DIRECTION ( 'NONE',  ( -1.000000000000000000, 0.000000000000000000, 0.000000000000000000 ) ) ;
#7613 = CARTESIAN_POINT ( 'NONE',  ( -54.99999999999999289, 0.000000000000000000, 0.000000000000000000 ) ) ;
#7614 = ADVANCED_FACE ( 'NONE', ( #3689 ), #9599, .F. ) ;
#7615 = LINE ( 'NONE', #1832, #8771 ) ;
#7616 = CARTESIAN_POINT ( 'NONE',  ( 41.77500000054622831, 20.00000000000000355, 98.07665518445361386 ) ) ;
#7617 = CARTESIAN_POINT ( 'NONE',  ( 28.37500000054622618, 12.34168156654572535, 90.79316153445363113 ) ) ;
#7618 = CARTESIAN_POINT ( 'NONE',  ( 26.89999999999998792, 17.56310227825321135, 83.29316153445363113 ) ) ;
#7619 = CARTESIAN_POINT ( 'NONE',  ( -50.00000000000001421, 20.00000000000000000, 137.5000000000000000 ) ) ;
#7620 = CARTESIAN_POINT ( 'NONE',  ( 37.07500000054622546, 26.19570976099943493, 86.29171490190961435 ) ) ;
#7621 = ORIENTED_EDGE ( 'NONE', *, *, #5224, .T. ) ;
#7622 = EDGE_CURVE ( 'NONE', #10986, #8335, #5349, .T. ) ;
#7623 = CARTESIAN_POINT ( 'NONE',  ( 46.57500000054622546, 15.71886984736413773, 84.90069139318163138 ) ) ;
#7624 = CARTESIAN_POINT ( 'NONE',  ( -4.967050660446461485, 49.34001764944455459, -20.40423414033599059 ) ) ;
#7625 = ORIENTED_EDGE ( 'NONE', *, *, #10505, .F. ) ;
#7626 = LINE ( 'NONE', #6724, #10156 ) ;
#7627 = ORIENTED_EDGE ( 'NONE', *, *, #6675, .T. ) ;
#7628 = AXIS2_PLACEMENT_3D ( 'NONE', #11973, #2134, #2269 ) ;
#7629 =( BOUNDED_CURVE ( )  B_SPLINE_CURVE ( 3, ( #9502, #7657, #1875, #11521 ),
 .UNSPECIFIED., .F., .F. ) 
 B_SPLINE_CURVE_WITH_KNOTS ( ( 4, 4 ),
 ( 4.712388980384689674, 6.013252511346182771 ),
 .UNSPECIFIED. ) 
 CURVE ( )  GEOMETRIC_REPRESENTATION_ITEM ( )  RATIONAL_B_SPLINE_CURVE ( ( 1.000000000000000000, 0.8638816171694809753, 0.8638816171694809753, 1.000000000000000000 ) ) 
 REPRESENTATION_ITEM ( '' )  );
#7630 = CARTESIAN_POINT ( 'NONE',  ( 41.75000000109246656, 17.56310227825320425, 98.29316153445363113 ) ) ;
#7631 = DIRECTION ( 'NONE',  ( 0.000000000000000000, 0.000000000000000000, -1.000000000000000000 ) ) ;
#7632 = CARTESIAN_POINT ( 'NONE',  ( 3.050317456283809570, 46.02489861342813526, -27.83468043274920234 ) ) ;
#7633 = CARTESIAN_POINT ( 'NONE',  ( 41.77500000054621410, 22.36655054427230027, 98.07665518445361386 ) ) ;
#7634 = PLANE ( 'NONE',  #11046 ) ;
#7635 = CARTESIAN_POINT ( 'NONE',  ( 47.39999999999999147, 27.13292387221364876, 88.47553407664153724 ) ) ;
#7636 = VECTOR ( 'NONE', #9323, 1000.000000000000000 ) ;
#7637 = CARTESIAN_POINT ( 'NONE',  ( -4.461205683540790723, 28.97367431253432812, -24.60633856694852994 ) ) ;
#7638 = CARTESIAN_POINT ( 'NONE',  ( 38.65000000109246514, 20.00000000000000355, 83.29316153445364534 ) ) ;
#7639 = ORIENTED_EDGE ( 'NONE', *, *, #10029, .F. ) ;
#7640 = CARTESIAN_POINT ( 'NONE',  ( 37.05000000109246372, 27.13292387221364876, 88.47553407664153724 ) ) ;
#7641 = CARTESIAN_POINT ( 'NONE',  ( 24.39999999999998792, 12.86707612778636012, 93.11078899226572503 ) ) ;
#7642 = ORIENTED_EDGE ( 'NONE', *, *, #7131, .F. ) ;
#7643 = CARTESIAN_POINT ( 'NONE',  ( -6.999999999999978684, 20.00000000000000355, 109.9999999999999858 ) ) ;
#7644 = ORIENTED_EDGE ( 'NONE', *, *, #6731, .F. ) ;
#7645 = DIRECTION ( 'NONE',  ( 0.000000000000000000, 0.000000000000000000, -1.000000000000000000 ) ) ;
#7646 = TOROIDAL_SURFACE ( 'NONE', #6024, 8.400000000000000355, 0.5999999999999999778 ) ;
#7647 = CARTESIAN_POINT ( 'NONE',  ( 1.328610784013299906, 10.08300648071286254, -20.96057967355971385 ) ) ;
#7648 = DIRECTION ( 'NONE',  ( -1.000000000000000000, -0.000000000000000000, -0.000000000000000000 ) ) ;
#7649 = CARTESIAN_POINT ( 'NONE',  ( 6.000000000000000000, 5.258101095580058680E-15, 5.057500000000000107 ) ) ;
#7650 = ORIENTED_EDGE ( 'NONE', *, *, #2314, .T. ) ;
#7651 = CARTESIAN_POINT ( 'NONE',  ( -8.665812433443574132E-16, 55.00000000000000000, -28.00000000000000355 ) ) ;
#7652 = CARTESIAN_POINT ( 'NONE',  ( 0.000000000000000000, 20.00000000000000355, 109.9999999999999858 ) ) ;
#7653 = CARTESIAN_POINT ( 'NONE',  ( 20.47500000054622760, 13.80429023900056684, 86.29171490190961435 ) ) ;
#7654 = AXIS2_PLACEMENT_3D ( 'NONE', #904, #8516, #10350 ) ;
#7655 = ORIENTED_EDGE ( 'NONE', *, *, #8549, .T. ) ;
#7656 = EDGE_CURVE ( 'NONE', #7533, #2987, #3818, .T. ) ;
#7657 = CARTESIAN_POINT ( 'NONE',  ( -23.99529484836403270, 27.49999999999999645, 148.5047051516359318 ) ) ;
#7658 = CYLINDRICAL_SURFACE ( 'NONE', #234, 7.500000000000000000 ) ;
#7659 = ORIENTED_EDGE ( 'NONE', *, *, #8095, .F. ) ;
#7660 = ORIENTED_EDGE ( 'NONE', *, *, #10849, .F. ) ;
#7661 = CIRCLE ( 'NONE', #10904, 5.057500000000000107 ) ;
#7662 = CARTESIAN_POINT ( 'NONE',  ( -7.933240127388049068, 26.09654486848563337, -19.44510781892114437 ) ) ;
#7663 = DIRECTION ( 'NONE',  ( 0.000000000000000000, 0.000000000000000000, 1.000000000000000000 ) ) ;
#7664 = CARTESIAN_POINT ( 'NONE',  ( 22.57500000054622902, 15.71886984736413773, 84.90069139318163138 ) ) ;
#7665 = DIRECTION ( 'NONE',  ( 1.000000000000000000, 0.000000000000000000, 0.000000000000000000 ) ) ;
#7666 = DIRECTION ( 'NONE',  ( 0.000000000000000000, -1.000000000000000000, 1.039664082171044875E-15 ) ) ;
#7667 = CARTESIAN_POINT ( 'NONE',  ( 90.00000000000000000, 0.000000000000000000, 0.000000000000000000 ) ) ;
#7668 = DIRECTION ( 'NONE',  ( -0.000000000000000000, -1.000000000000000000, -0.000000000000000000 ) ) ;
#7669 = CIRCLE ( 'NONE', #2599, 8.000000000000000000 ) ;
#7670 = CARTESIAN_POINT ( 'NONE',  ( 19.99999999999999645, 20.00000000000000355, 170.0000119999999697 ) ) ;
#7671 = ORIENTED_EDGE ( 'NONE', *, *, #189, .T. ) ;
#7672 = CARTESIAN_POINT ( 'NONE',  ( -3.241172199251822317, 10.51724913471846889, -27.81845307868313100 ) ) ;
#7673 = EDGE_CURVE ( 'NONE', #174, #938, #7569, .T. ) ;
#7674 = CONTEXT_DEPENDENT_SHAPE_REPRESENTATION ( #3023, #7103 ) ;
#7675 = B_SPLINE_CURVE_WITH_KNOTS ( 'NONE', 3,
 ( #2777, #12483, #2841, #11596, #6769, #8047, #11915, #7023, #1201, #7792, #3158, #9698, #10897, #7981, #11664, #3089, #1947, #6956, #3222, #247 ),
 .UNSPECIFIED., .F., .F.,
 ( 4, 2, 2, 2, 2, 2, 2, 2, 2, 4 ),
 ( 0.01567185795944686308, 0.01665140573566027682, 0.01763095351187368709, 0.01812072739998039222, 0.01861050128808709736, 0.01959004906430051110, 0.02056959684051392484, 0.02154914461672733511, 0.02252869239294074538, 0.02350824016915415912 ),
 .UNSPECIFIED. ) ;
#7676 = CARTESIAN_POINT ( 'NONE',  ( 25.57500000054621836, 26.19570976099943849, 95.29460816699764791 ) ) ;
#7677 = LINE ( 'NONE', #11359, #7349 ) ;
#7678 = ADVANCED_FACE ( 'NONE', ( #6488 ), #3568, .T. ) ;
#7679 = CARTESIAN_POINT ( 'NONE',  ( 40.57500000054623257, 15.71886984736413773, 84.90069139318163138 ) ) ;
#7680 = AXIS2_PLACEMENT_3D ( 'NONE', #12217, #3519, #3958 ) ;
#7681 = CARTESIAN_POINT ( 'NONE',  ( 25.67500000054622333, 24.28113015263587116, 96.68563167572563088 ) ) ;
#7682 = CARTESIAN_POINT ( 'NONE',  ( 29.69999999999998508, 26.37988106264029398, 95.42841645007781892 ) ) ;
#7683 =( NAMED_UNIT ( * ) SI_UNIT ( $, .STERADIAN. ) SOLID_ANGLE_UNIT ( ) );
#7684 = CARTESIAN_POINT ( 'NONE',  ( 31.77500000054622831, 20.00000000000000355, 98.07665518445361386 ) ) ;
#7685 = ORIENTED_EDGE ( 'NONE', *, *, #6783, .F. ) ;
#7686 = FACE_OUTER_BOUND ( 'NONE', #1207, .T. ) ;
#7687 = VERTEX_POINT ( 'NONE', #2805 ) ;
#7688 = VECTOR ( 'NONE', #11353, 1000.000000000000000 ) ;
#7689 = CARTESIAN_POINT ( 'NONE',  ( 5.844014480200539374, 11.87882549901748241, 20.17240906330831507 ) ) ;
#7690 = ORIENTED_EDGE ( 'NONE', *, *, #5232, .T. ) ;
#7691 = AXIS2_PLACEMENT_3D ( 'NONE', #3320, #10939, #9866 ) ;
#7692 = PLANE ( 'NONE',  #8304 ) ;
#7693 = CARTESIAN_POINT ( 'NONE',  ( 27.49999999999999645, 20.00000000000000355, 170.9999999999999716 ) ) ;
#7694 = CARTESIAN_POINT ( 'NONE',  ( -31.74999999999995737, 0.000000000000000000, 0.000000000000000000 ) ) ;
#7695 = EDGE_CURVE ( 'NONE', #8919, #223, #2748, .T. ) ;
#7696 = DIRECTION ( 'NONE',  ( 0.000000000000000000, 0.000000000000000000, 1.000000000000000000 ) ) ;
#7697 = CARTESIAN_POINT ( 'NONE',  ( 19.87500000054622262, 20.00000000000000355, 98.07665518445361386 ) ) ;
#7698 = CARTESIAN_POINT ( 'NONE',  ( -7.533608174404544222, 26.60766787979761006, -23.84262432367340523 ) ) ;
#7699 = CARTESIAN_POINT ( 'NONE',  ( 49.27500000054623541, 27.65831843345427998, 90.79316153445363113 ) ) ;
#7700 = ORIENTED_EDGE ( 'NONE', *, *, #10391, .T. ) ;
#7701 = CARTESIAN_POINT ( 'NONE',  ( 33.05000000109247082, 27.13292387221364876, 88.47553407664153724 ) ) ;
#7702 = CARTESIAN_POINT ( 'NONE',  ( 24.59999999999998721, 12.86707612778636012, 88.47553407664152303 ) ) ;
#7703 = VERTEX_POINT ( 'NONE', #10540 ) ;
#7705 = EDGE_CURVE ( 'NONE', #10754, #4846, #10287, .T. ) ;
#7704 =( BOUNDED_CURVE ( )  B_SPLINE_CURVE ( 2, ( #2494, #11248, #6370, #5422, #10236, #7378, #599, #4461, #8340, #12206, #3506 ),
 .UNSPECIFIED., .F., .F. ) 
 B_SPLINE_CURVE_WITH_KNOTS ( ( 3, 2, 2, 2, 2, 3 ),
 ( 0.5666666666666666519, 0.5733333333333333615, 0.5799999999999999600, 0.5866666666666666696, 0.5933333333333333792, 0.5999999999999999778 ),
 .UNSPECIFIED. ) 
 CURVE ( )  GEOMETRIC_REPRESENTATION_ITEM ( )  RATIONAL_B_SPLINE_CURVE ( ( 1.000000000000000000, 0.9510565162951535312, 1.000000000000000000, 0.9510565162951535312, 1.000000000000000000, 0.9510565162951535312, 1.000000000000000000, 0.9510565162951535312, 1.000000000000000000, 0.9510565162951535312, 1.000000000000000000 ) ) 
 REPRESENTATION_ITEM ( '' )  );
#7706 = VERTEX_POINT ( 'NONE', #10597 ) ;
#7707 = CIRCLE ( 'NONE', #8317, 6.999999999999964473 ) ;
#7708 = CARTESIAN_POINT ( 'NONE',  ( -6.108719317430274742, 27.92396576624410187, -24.24357326025485193 ) ) ;
#7709 = CARTESIAN_POINT ( 'NONE',  ( 8.962973916282662046, 15.55345101320112455, -18.99194879768439037 ) ) ;
#7710 = CARTESIAN_POINT ( 'NONE',  ( -1.322864546895947679, 29.91770977471893289, 24.96717945133217498 ) ) ;
#7711 = CARTESIAN_POINT ( 'NONE',  ( 34.27500000054623541, 12.34168156654572535, 90.79316153445363113 ) ) ;
#7712 = DIRECTION ( 'NONE',  ( 0.000000000000000000, 0.000000000000000000, 1.000000000000000000 ) ) ;
#7713 = FACE_OUTER_BOUND ( 'NONE', #2290, .T. ) ;
#7714 = CARTESIAN_POINT ( 'NONE',  ( 27.50000000000000355, 27.49999999999999645, 145.0000000000000000 ) ) ;
#7715 = ORIENTED_EDGE ( 'NONE', *, *, #10215, .T. ) ;
#7716 = AXIS2_PLACEMENT_3D ( 'NONE', #125, #11731, #11669 ) ;
#7717 = CARTESIAN_POINT ( 'NONE',  ( 0.000000000000000000, -4.262400816306111331E-15, 0.000000000000000000 ) ) ;
#7718 = CARTESIAN_POINT ( 'NONE',  ( -2.000000000000015543, 20.00000000000000355, 90.79316153445363113 ) ) ;
#7719 = CARTESIAN_POINT ( 'NONE',  ( 19.77500000054622831, 20.00000000000000355, 98.07665518445361386 ) ) ;
#7720 = EDGE_LOOP ( 'NONE', ( #8316, #6190, #1454, #2876 ) ) ;
#7721 = CARTESIAN_POINT ( 'NONE',  ( 45.65000000109247225, 20.00000000000000355, 98.29316153445363113 ) ) ;
#7722 = UNCERTAINTY_MEASURE_WITH_UNIT (LENGTH_MEASURE( 1.000000000000000082E-05 ), #5192, 'distance_accuracy_value', 'NONE');
#7723 = CARTESIAN_POINT ( 'NONE',  ( 3.307665144821749337, 53.76359313335627377, -20.73917751733423742 ) ) ;
#7724 = EDGE_LOOP ( 'NONE', ( #10553, #572, #1615, #4771, #3830, #1761 ) ) ;
#7725 = ORIENTED_EDGE ( 'NONE', *, *, #10992, .F. ) ;
#7726 = AXIS2_PLACEMENT_3D ( 'NONE', #6363, #408, #10285 ) ;
#7727 = DIRECTION ( 'NONE',  ( -0.000000000000000000, -1.000000000000000000, -0.000000000000000000 ) ) ;
#7728 = EDGE_CURVE ( 'NONE', #4738, #9626, #8581, .T. ) ;
#7729 = DIRECTION ( 'NONE',  ( -0.000000000000000000, -1.000000000000000000, -0.000000000000000000 ) ) ;
#7730 = CARTESIAN_POINT ( 'NONE',  ( 0.000000000000000000, 0.000000000000000000, -25.00000000000000000 ) ) ;
#7731 = DIRECTION ( 'NONE',  ( -0.000000000000000000, 0.000000000000000000, 1.000000000000000000 ) ) ;
#7732 = CARTESIAN_POINT ( 'NONE',  ( 27.49999999999999645, 20.00000000000000355, 189.9999999999999716 ) ) ;
#7733 = CARTESIAN_POINT ( 'NONE',  ( -2.000000000000015543, 20.00000000000000355, 98.29316153445363113 ) ) ;
#7734 = CARTESIAN_POINT ( 'NONE',  ( 8.648708627877683242, 25.03051607003104095, -19.13710648617777466 ) ) ;
#7735 = CARTESIAN_POINT ( 'NONE',  ( 7.927224944456558120, 13.89552811154835510, 23.71088769051724654 ) ) ;
#7736 = VERTEX_POINT ( 'NONE', #7506 ) ;
#7737 = CARTESIAN_POINT ( 'NONE',  ( -31.74999999999995737, 0.000000000000000000, 9.000000000000000000 ) ) ;
#7738 = ADVANCED_FACE ( 'NONE', ( #841 ), #5794, .F. ) ;
#7739 = CARTESIAN_POINT ( 'NONE',  ( 28.67500000054622689, 15.71886984736413773, 84.90069139318163138 ) ) ;
#7740 = CARTESIAN_POINT ( 'NONE',  ( 48.17500000054622689, 13.80429023900056507, 95.29460816699764791 ) ) ;
#7741 = CARTESIAN_POINT ( 'NONE',  ( 42.27500000054622120, 12.34168156654572357, 90.79316153445363113 ) ) ;
#7742 = CARTESIAN_POINT ( 'NONE',  ( 26.27500000054622475, 13.07298590277314254, 93.04388485072563242 ) ) ;
#7743 = CARTESIAN_POINT ( 'NONE',  ( 25.79999999999998650, 24.40838939219354842, 96.86078899226572503 ) ) ;
#7744 = ADVANCED_FACE ( 'NONE', ( #11377 ), #8398, .F. ) ;
#7745 = CARTESIAN_POINT ( 'NONE',  ( 35.57500000054622546, 24.28113015263587116, 96.68563167572563088 ) ) ;
#7746 = ORIENTED_EDGE ( 'NONE', *, *, #4509, .T. ) ;
#7747 = CARTESIAN_POINT ( 'NONE',  ( -31.74999999999995737, 0.000000000000000000, 0.000000000000000000 ) ) ;
#7748 = ORIENTED_EDGE ( 'NONE', *, *, #3535, .T. ) ;
#7749 = CARTESIAN_POINT ( 'NONE',  ( 0.6519265100557631865, 54.96824252967201119, 27.99427508789008812 ) ) ;
#7750 = VERTEX_POINT ( 'NONE', #11437 ) ;
#7751 = CARTESIAN_POINT ( 'NONE',  ( 43.49999999999998579, 27.88596668178699645, 90.79316153445363113 ) ) ;
#7752 = DIRECTION ( 'NONE',  ( 0.000000000000000000, -0.4999999999999985012, 0.8660254037844394848 ) ) ;
#7753 = CARTESIAN_POINT ( 'NONE',  ( 43.27500000054622120, 26.92701409722686634, 88.54243821818162985 ) ) ;
#7754 = CARTESIAN_POINT ( 'NONE',  ( 40.65000000109246514, 20.00000000000000355, 83.29316153445364534 ) ) ;
#7755 = LINE ( 'NONE', #8354, #2568 ) ;
#7756 = CARTESIAN_POINT ( 'NONE',  ( 46.17500000054622689, 13.80429023900056507, 95.29460816699764791 ) ) ;
#7757 = CARTESIAN_POINT ( 'NONE',  ( 47.49999999999997868, 27.88596668178699645, 90.79316153445363113 ) ) ;
#7758 = EDGE_CURVE ( 'NONE', #5293, #10986, #2715, .T. ) ;
#7759 = CARTESIAN_POINT ( 'NONE',  ( 40.99999999999998579, 20.00000000000000355, 83.29316153445364534 ) ) ;
#7760 = DIRECTION ( 'NONE',  ( 0.000000000000000000, -0.000000000000000000, 1.000000000000000000 ) ) ;
#7761 = ORIENTED_EDGE ( 'NONE', *, *, #3642, .T. ) ;
#7762 = CIRCLE ( 'NONE', #4308, 7.499999999999992895 ) ;
#7763 = CARTESIAN_POINT ( 'NONE',  ( 33.85000000109246798, 15.59161060780645691, 96.86078899226572503 ) ) ;
#7764 = LINE ( 'NONE', #4975, #6286 ) ;
#7765 = ORIENTED_EDGE ( 'NONE', *, *, #5297, .T. ) ;
#7766 = EDGE_CURVE ( 'NONE', #11262, #8158, #8519, .T. ) ;
#7767 = ORIENTED_EDGE ( 'NONE', *, *, #6076, .T. ) ;
#7768 = FACE_OUTER_BOUND ( 'NONE', #2827, .T. ) ;
#7769 = LINE ( 'NONE', #9740, #7853 ) ;
#7770 = CARTESIAN_POINT ( 'NONE',  ( 12.59999999999999964, 0.000000000000000000, 0.000000000000000000 ) ) ;
#7771 = AXIS2_PLACEMENT_3D ( 'NONE', #2012, #1139, #8049 ) ;
#7772 = EDGE_CURVE ( 'NONE', #11952, #8287, #10475, .T. ) ;
#7773 = CARTESIAN_POINT ( 'NONE',  ( 34.17500000054622689, 13.07298590277314254, 93.04388485072563242 ) ) ;
#7774 = CARTESIAN_POINT ( 'NONE',  ( 40.57500000054621836, 13.80429023900056684, 86.29171490190961435 ) ) ;
#7775 = B_SPLINE_CURVE_WITH_KNOTS ( 'NONE', 3,
 ( #6486, #10083, #1907, #4962, #10857, #4066, #7945, #2868, #5791, #5916, #5263, #2931, #7879, #8824, #144, #8892, #11749, #8761, #9134, #2993, #3816, #6728, #6860, #5028, #10723, #6795 ),
 .UNSPECIFIED., .F., .F.,
 ( 4, 2, 2, 2, 2, 2, 2, 2, 2, 2, 2, 2, 4 ),
 ( 0.01576884472483168140, 0.01675373746250873042, 0.01773863020018578290, 0.01970841567553989482, 0.02167820115089400673, 0.02266309388857106616, 0.02364798662624812906, 0.02561777210160225138, 0.02660266483927931427, 0.02758755757695637717, 0.02955734305231050643, 0.03054223578998756933, 0.03152712852766463569 ),
 .UNSPECIFIED. ) ;
#7776 = CARTESIAN_POINT ( 'NONE',  ( 34.95000000109246940, 26.37988106264029398, 86.15790661882942914 ) ) ;
#7777 = CARTESIAN_POINT ( 'NONE',  ( 10.00000000000000355, 20.00000000000000355, -26.15339366124404208 ) ) ;
#7778 = DIRECTION ( 'NONE',  ( -1.000000000000000000, -0.000000000000000000, -0.000000000000000000 ) ) ;
#7779 = VERTEX_POINT ( 'NONE', #5977 ) ;
#7780 = CARTESIAN_POINT ( 'NONE',  ( 48.95000000109246940, 26.37988106264029398, 86.15790661882942914 ) ) ;
#7781 = ADVANCED_FACE ( 'NONE', ( #9852 ), #4136, .T. ) ;
#7782 = ORIENTED_EDGE ( 'NONE', *, *, #4832, .F. ) ;
#7783 = CARTESIAN_POINT ( 'NONE',  ( 35.99999999999999289, 20.00000000000000355, 98.29316153445363113 ) ) ;
#7784 = VECTOR ( 'NONE', #3644, 1000.000000000000000 ) ;
#7785 = CARTESIAN_POINT ( 'NONE',  ( -5.000000000000000000, 50.00000000000000000, 27.54995462791182348 ) ) ;
#7786 = VERTEX_POINT ( 'NONE', #2100 ) ;
#7787 = AXIS2_PLACEMENT_3D ( 'NONE', #7732, #754, #3723 ) ;
#7788 = ORIENTED_EDGE ( 'NONE', *, *, #11328, .F. ) ;
#7789 = CARTESIAN_POINT ( 'NONE',  ( 3.061616997868383043E-15, 0.000000000000000000, 25.00000000000000000 ) ) ;
#7790 = CARTESIAN_POINT ( 'NONE',  ( 6.000000000000000000, 5.839897972853065333, -6.938893903907228378E-15 ) ) ;
#7791 = CARTESIAN_POINT ( 'NONE',  ( 8.665638667393702477, 24.99499069331186973, 85.19347117998894703 ) ) ;
#7792 = CARTESIAN_POINT ( 'NONE',  ( 3.052678183968668524, 46.02654057254596154, -24.81443426854575307 ) ) ;
#7793 = DIRECTION ( 'NONE',  ( 0.000000000000000000, 0.000000000000000000, 1.000000000000000000 ) ) ;
#7794 = LINE ( 'NONE', #11666, #11819 ) ;
#7795 = CARTESIAN_POINT ( 'NONE',  ( 2.504536724946392567, 45.66016527775391154, 27.88910086977369573 ) ) ;
#7796 = DIRECTION ( 'NONE',  ( -1.000000000000000000, -0.000000000000000000, -0.000000000000000000 ) ) ;
#7797 = VERTEX_POINT ( 'NONE', #9916 ) ;
#7798 = DIRECTION ( 'NONE',  ( -0.000000000000000000, 0.000000000000000000, 1.000000000000000000 ) ) ;
#7799 = APPLICATION_PROTOCOL_DEFINITION ( 'draft international standard', 'automotive_design', 1998, #12179 ) ;
#7800 = MECHANICAL_DESIGN_GEOMETRIC_PRESENTATION_REPRESENTATION (  '', ( #923 ), #3741 ) ;
#7801 = APPLICATION_CONTEXT ( 'automotive_design' ) ;
#7802 = CARTESIAN_POINT ( 'NONE',  ( 24.07500000054622546, 15.71886984736413417, 96.68563167572563088 ) ) ;
#7803 = CARTESIAN_POINT ( 'NONE',  ( 48.87500000054622262, 20.00000000000000355, 83.50966788445364841 ) ) ;
#7804 = CARTESIAN_POINT ( 'NONE',  ( 38.07500000054622546, 13.80429023900056507, 95.29460816699764791 ) ) ;
#7805 = CARTESIAN_POINT ( 'NONE',  ( 22.77500000054622475, 17.63344945572770328, 83.50966788445364841 ) ) ;
#7806 = CARTESIAN_POINT ( 'NONE',  ( 22.79999999999998650, 15.59161060780646046, 84.72553407664153724 ) ) ;
#7807 = CARTESIAN_POINT ( 'NONE',  ( 35.17500000054622689, 26.92701409722686634, 88.54243821818162985 ) ) ;
#7808 = ORIENTED_EDGE ( 'NONE', *, *, #2948, .T. ) ;
#7809 = DIRECTION ( 'NONE',  ( -1.000000000000000000, 0.000000000000000000, -0.000000000000000000 ) ) ;
#7810 = ORIENTED_EDGE ( 'NONE', *, *, #598, .T. ) ;
#7811 = EDGE_CURVE ( 'NONE', #2249, #11209, #4960, .T. ) ;
#7812 = CARTESIAN_POINT ( 'NONE',  ( 3.764387367674736140, 53.30686585430343172, 27.74677055206694121 ) ) ;
#7813 = ORIENTED_EDGE ( 'NONE', *, *, #3207, .F. ) ;
#7814 =( LENGTH_UNIT ( ) NAMED_UNIT ( * ) SI_UNIT ( .MILLI., .METRE. ) );
#7815 = CARTESIAN_POINT ( 'NONE',  ( 42.99999999999999289, 20.00000000000000355, 83.29316153445364534 ) ) ;
#7816 = AXIS2_PLACEMENT_3D ( 'NONE', #4420, #6391, #12168 ) ;
#7817 = LINE ( 'NONE', #5854, #2973 ) ;
#7818 = ADVANCED_FACE ( 'NONE', ( #17 ), #9582, .F. ) ;
#7819 = CARTESIAN_POINT ( 'NONE',  ( 38.97500000054622404, 22.36655054427230382, 83.50966788445364841 ) ) ;
#7820 = CARTESIAN_POINT ( 'NONE',  ( 39.65000000109246514, 20.00000000000000355, 98.29316153445363113 ) ) ;
#7821 = CARTESIAN_POINT ( 'NONE',  ( 27.49999999999999645, 20.00000000000000355, 188.9999999999999716 ) ) ;
#7822 =( BOUNDED_CURVE ( )  B_SPLINE_CURVE ( 2, ( #1047, #2874, #3063, #3822, #217, #8767, #4843, #11816, #1103, #4971, #5861 ),
 .UNSPECIFIED., .F., .F. ) 
 B_SPLINE_CURVE_WITH_KNOTS ( ( 3, 2, 2, 2, 2, 3 ),
 ( 0.3333333333333333703, 0.3400000000000000799, 0.3466666666666667340, 0.3533333333333333881, 0.3600000000000000422, 0.3666666666666666963 ),
 .UNSPECIFIED. ) 
 CURVE ( )  GEOMETRIC_REPRESENTATION_ITEM ( )  RATIONAL_B_SPLINE_CURVE ( ( 0.9999999999999995559, 0.9510565162951539753, 1.000000000000000000, 0.9510565162951535312, 1.000000000000000000, 0.9510565162951535312, 1.000000000000000000, 0.9510565162951535312, 1.000000000000000000, 0.9510565162951530871, 1.000000000000000444 ) ) 
 REPRESENTATION_ITEM ( '' )  );
#7823 = CARTESIAN_POINT ( 'NONE',  ( 44.27500000054622120, 13.07298590277314254, 93.04388485072563242 ) ) ;
#7824 = CARTESIAN_POINT ( 'NONE',  ( 45.09999999999999432, 22.43689772174679575, 83.29316153445363113 ) ) ;
#7825 = CARTESIAN_POINT ( 'NONE',  ( 0.000000000000000000, 0.000000000000000000, 0.000000000000000000 ) ) ;
#7826 = PLANE ( 'NONE',  #5048 ) ;
#7827 = ORIENTED_EDGE ( 'NONE', *, *, #11650, .T. ) ;
#7828 = CARTESIAN_POINT ( 'NONE',  ( 32.25000000109245946, 12.86707612778636012, 88.47553407664152303 ) ) ;
#7829 = CARTESIAN_POINT ( 'NONE',  ( -5.038456156925416707, 11.33776630238819116, 24.49323865847078707 ) ) ;
#7830 = ORIENTED_EDGE ( 'NONE', *, *, #5433, .F. ) ;
#7831 = ORIENTED_EDGE ( 'NONE', *, *, #7705, .T. ) ;
#7832 = DIRECTION ( 'NONE',  ( 1.000000000000000000, -0.000000000000000000, -0.000000000000000000 ) ) ;
#7833 = ADVANCED_FACE ( 'NONE', ( #11689, #2995 ), #8827, .T. ) ;
#7834 = DIRECTION ( 'NONE',  ( -0.000000000000000000, -0.000000000000000000, 1.000000000000000000 ) ) ;
#7835 = CARTESIAN_POINT ( 'NONE',  ( 48.39999999999999147, 12.86707612778636012, 93.11078899226572503 ) ) ;
#7836 = VECTOR ( 'NONE', #11154, 1000.000000000000114 ) ;
#7837 = CARTESIAN_POINT ( 'NONE',  ( 38.07500000054623257, 13.80429023900056507, 95.29460816699764791 ) ) ;
#7838 = CARTESIAN_POINT ( 'NONE',  ( 33.27500000054622831, 26.92701409722686634, 88.54243821818162985 ) ) ;
#7839 = CARTESIAN_POINT ( 'NONE',  ( 35.35000000109246088, 26.37988106264029398, 95.42841645007781892 ) ) ;
#7840 = DIRECTION ( 'NONE',  ( -1.000000000000000000, 0.000000000000000000, 0.000000000000000000 ) ) ;
#7841 = DIRECTION ( 'NONE',  ( 1.000000000000000000, -0.000000000000000000, -0.000000000000000000 ) ) ;
#7842 = ORIENTED_EDGE ( 'NONE', *, *, #10377, .T. ) ;
#7843 = CARTESIAN_POINT ( 'NONE',  ( 3.761098173404043621, 53.29862245996868353, -24.71568690466639140 ) ) ;
#7844 = CARTESIAN_POINT ( 'NONE',  ( 0.000000000000000000, 2.919948986426540660, 5.057499999999996554 ) ) ;
#7845 = EDGE_LOOP ( 'NONE', ( #9113, #8003, #8087 ) ) ;
#7846 = CARTESIAN_POINT ( 'NONE',  ( 0.000000000000000000, -2.919948986426523341, 5.057500000000002771 ) ) ;
#7847 = ORIENTED_EDGE ( 'NONE', *, *, #3967, .T. ) ;
#7848 = AXIS2_PLACEMENT_3D ( 'NONE', #942, #7472, #3851 ) ;
#7849 = EDGE_CURVE ( 'NONE', #6810, #4582, #5031, .T. ) ;
#7850 = ORIENTED_EDGE ( 'NONE', *, *, #6451, .F. ) ;
#7851 = DIRECTION ( 'NONE',  ( 0.000000000000000000, -0.5000000000000012212, -0.8660254037844380415 ) ) ;
#7852 = ADVANCED_FACE ( 'NONE', ( #6862 ), #8895, .F. ) ;
#7853 = VECTOR ( 'NONE', #11641, 1000.000000000000114 ) ;
#7854 = CARTESIAN_POINT ( 'NONE',  ( 8.035266039410178252, 25.95549721022405976, 95.35796119567172013 ) ) ;
#7855 = CARTESIAN_POINT ( 'NONE',  ( -50.00000000000001421, 84.49999999999998579, 101.8533255156881978 ) ) ;
#7856 = DIRECTION ( 'NONE',  ( 1.000000000000000000, 0.000000000000000000, 0.000000000000000000 ) ) ;
#7857 = FACE_OUTER_BOUND ( 'NONE', #7861, .T. ) ;
#7858 = CARTESIAN_POINT ( 'NONE',  ( -21.00000000000001776, 72.60660171779821326, 154.3533255156881694 ) ) ;
#7859 = CARTESIAN_POINT ( 'NONE',  ( 45.17500000054622689, 26.92701409722686634, 88.54243821818162985 ) ) ;
#7860 = CARTESIAN_POINT ( 'NONE',  ( 8.123360751522579193, 14.15902104166613107, 23.64419573351483450 ) ) ;
#7861 = EDGE_LOOP ( 'NONE', ( #5311, #7746, #9412, #4473 ) ) ;
#7862 = EDGE_CURVE ( 'NONE', #1674, #9180, #1879, .T. ) ;
#7863 = CARTESIAN_POINT ( 'NONE',  ( -1.312971999154120883, 10.08108238931077238, -27.97112805829059212 ) ) ;
#7864 = APPLICATION_PROTOCOL_DEFINITION ( 'draft international standard', 'automotive_design', 1998, #5622 ) ;
#7865 = CARTESIAN_POINT ( 'NONE',  ( 45.99999999999998579, 20.00000000000000355, 98.29316153445363113 ) ) ;
#7866 = CARTESIAN_POINT ( 'NONE',  ( 48.37500000054621552, 12.34168156654572535, 90.79316153445363113 ) ) ;
#7867 = CARTESIAN_POINT ( 'NONE',  ( 32.77500000054622831, 20.00000000000000355, 83.50966788445364841 ) ) ;
#7868 = CIRCLE ( 'NONE', #1187, 5.057500000000000107 ) ;
#7869 = CARTESIAN_POINT ( 'NONE',  ( 22.27500000054622120, 13.07298590277314254, 93.04388485072563242 ) ) ;
#7870 = CARTESIAN_POINT ( 'NONE',  ( 22.19999999999998863, 15.59161060780645691, 96.86078899226572503 ) ) ;
#7871 = CARTESIAN_POINT ( 'NONE',  ( 6.000000000000000000, 2.919948986426540660, 5.057499999999996554 ) ) ;
#7872 = CARTESIAN_POINT ( 'NONE',  ( 30.97500000054622760, 24.28113015263587471, 84.90069139318163138 ) ) ;
#7873 = ORIENTED_EDGE ( 'NONE', *, *, #12097, .T. ) ;
#7874 = CARTESIAN_POINT ( 'NONE',  ( 5.000000000000000000, 4.685197434473814759, -5.637851296924623057E-15 ) ) ;
#7875 = ORIENTED_EDGE ( 'NONE', *, *, #12257, .F. ) ;
#7876 = CARTESIAN_POINT ( 'NONE',  ( 32.00000000000000000, 0.000000000000000000, 0.000000000000000000 ) ) ;
#7877 = ORIENTED_EDGE ( 'NONE', *, *, #1010, .F. ) ;
#7878 = DIRECTION ( 'NONE',  ( -0.000000000000000000, -0.000000000000000000, 1.000000000000000000 ) ) ;
#7879 = CARTESIAN_POINT ( 'NONE',  ( 7.296171710155400447, 13.15373968915042546, -27.03372408122936221 ) ) ;
#7880 = CARTESIAN_POINT ( 'NONE',  ( 41.07500000054622546, 24.28113015263587471, 84.90069139318163138 ) ) ;
#7881 = DIRECTION ( 'NONE',  ( 1.000000000000000000, 0.000000000000000000, 0.000000000000000000 ) ) ;
#7882 = EDGE_CURVE ( 'NONE', #7590, #1159, #4518, .T. ) ;
#7883 = CARTESIAN_POINT ( 'NONE',  ( 20.25000000109246301, 12.86707612778636012, 88.47553407664152303 ) ) ;
#7884 = CARTESIAN_POINT ( 'NONE',  ( 41.59999999999998721, 27.13292387221364876, 93.11078899226573924 ) ) ;
#7885 = CARTESIAN_POINT ( 'NONE',  ( -9.659227801817477754, 22.60918507870266581, -23.05884188866823337 ) ) ;
#7886 = DIRECTION ( 'NONE',  ( 1.000000000000000000, 0.000000000000000000, 0.000000000000000000 ) ) ;
#7887 = VECTOR ( 'NONE', #6975, 1000.000000000000000 ) ;
#7888 = VERTEX_POINT ( 'NONE', #6921 ) ;
#7889 = CARTESIAN_POINT ( 'NONE',  ( 30.25000000109246656, 12.86707612778636012, 88.47553407664152303 ) ) ;
#7890 = CARTESIAN_POINT ( 'NONE',  ( 2.213389590484158731, 45.51360200414269741, -24.90224851187377553 ) ) ;
#7891 = ORIENTED_EDGE ( 'NONE', *, *, #12308, .T. ) ;
#7892 = AXIS2_PLACEMENT_3D ( 'NONE', #9181, #9119, #11971 ) ;
#7893 = EDGE_LOOP ( 'NONE', ( #4111, #3241, #10268, #1734 ) ) ;
#7894 = CARTESIAN_POINT ( 'NONE',  ( -34.72841614740047333, 18.00000000000000355, 170.0000119999999697 ) ) ;
#7895 = CARTESIAN_POINT ( 'NONE',  ( -5.000000000000000888, 18.00000000000000355, 218.7511230907454944 ) ) ;
#7896 = LINE ( 'NONE', #11766, #1696 ) ;
#7897 = CARTESIAN_POINT ( 'NONE',  ( 32.77500000054622831, 20.00000000000000355, 83.50966788445364841 ) ) ;
#7898 = CARTESIAN_POINT ( 'NONE',  ( 29.47500000054622404, 26.92701409722686634, 93.04388485072563242 ) ) ;
#7899 = CARTESIAN_POINT ( 'NONE',  ( -3.768914454385754897, 53.30204245436056709, 27.74617514008307850 ) ) ;
#7900 = FACE_OUTER_BOUND ( 'NONE', #394, .T. ) ;
#7901 = PLANE ( 'NONE',  #4826 ) ;
#7902 = ORIENTED_EDGE ( 'NONE', *, *, #10132, .F. ) ;
#7903 = EDGE_CURVE ( 'NONE', #5293, #5215, #5332, .T. ) ;
#7904 = CARTESIAN_POINT ( 'NONE',  ( 49.67500000054622689, 24.28113015263587116, 96.68563167572563088 ) ) ;
#7905 = CARTESIAN_POINT ( 'NONE',  ( 48.75000000109246656, 22.43689772174679575, 83.29316153445363113 ) ) ;
#7906 = EDGE_LOOP ( 'NONE', ( #10112, #10918, #12532, #5585 ) ) ;
#7907 = CYLINDRICAL_SURFACE ( 'NONE', #1536, 10.00000000000000355 ) ;
#7908 = VECTOR ( 'NONE', #4077, 1000.000000000000000 ) ;
#7909 = ORIENTED_EDGE ( 'NONE', *, *, #4213, .F. ) ;
#7910 = PRODUCT_DEFINITION ( 'UNKNOWN', '', #9203, #2187 ) ;
#7911 = CARTESIAN_POINT ( 'NONE',  ( 5.000000000000000000, -3.513898075855359071, 2.028750000000004494 ) ) ;
#7912 = CARTESIAN_POINT ( 'NONE',  ( -5.300214471940789096, 11.51392236371535382, -24.43326627631521220 ) ) ;
#7913 = ADVANCED_FACE ( 'NONE', ( #6797 ), #5918, .F. ) ;
#7914 = DIRECTION ( 'NONE',  ( 1.000000000000000000, 0.000000000000000000, 0.000000000000000000 ) ) ;
#7915 = VECTOR ( 'NONE', #757, 1000.000000000000000 ) ;
#7916 = FACE_OUTER_BOUND ( 'NONE', #3391, .T. ) ;
#7917 = CARTESIAN_POINT ( 'NONE',  ( 9.950222915369092647, 21.02923226400954704, 98.22668337568666175 ) ) ;
#7918 = CARTESIAN_POINT ( 'NONE',  ( 37.29999999999998295, 26.37988106264029398, 86.15790661882942914 ) ) ;
#7919 = CARTESIAN_POINT ( 'NONE',  ( 9.669242541481478881, 22.63421706188354676, 18.64209396758665349 ) ) ;
#7920 = LINE ( 'NONE', #11786, #4319 ) ;
#7921 = CARTESIAN_POINT ( 'NONE',  ( 5.000000000000000000, 50.00000000000000000, -28.00000000000000711 ) ) ;
#7922 = CARTESIAN_POINT ( 'NONE',  ( 40.47500000054622404, 13.80429023900056684, 86.29171490190961435 ) ) ;
#7923 = FACE_OUTER_BOUND ( 'NONE', #3971, .T. ) ;
#7924 = ORIENTED_EDGE ( 'NONE', *, *, #335, .F. ) ;
#7925 = AXIS2_PLACEMENT_3D ( 'NONE', #5338, #454, #5401 ) ;
#7926 = CARTESIAN_POINT ( 'NONE',  ( 2.611671490993349831, 29.65850121673988227, -24.86521292532985328 ) ) ;
#7927 = EDGE_CURVE ( 'NONE', #481, #9685, #11607, .T. ) ;
#7928 = CONTEXT_DEPENDENT_SHAPE_REPRESENTATION ( #9513, #11977 ) ;
#7929 = DIRECTION ( 'NONE',  ( -0.000000000000000000, -0.000000000000000000, 1.000000000000000000 ) ) ;
#7930 = EDGE_CURVE ( 'NONE', #7940, #11698, #3880, .T. ) ;
#7931 = CARTESIAN_POINT ( 'NONE',  ( 35.47500000054623115, 26.19570976099943849, 95.29460816699764791 ) ) ;
#7932 = ADVANCED_FACE ( 'NONE', ( #1043 ), #4903, .F. ) ;
#7933 = CARTESIAN_POINT ( 'NONE',  ( 6.615773601782837687, 12.47291401044366310, -24.11353245396511014 ) ) ;
#7934 = CARTESIAN_POINT ( 'NONE',  ( 22.59999999999998721, 12.86707612778636012, 88.47553407664152303 ) ) ;
#7935 = SURFACE_SIDE_STYLE ('',( #2228 ) ) ;
#7936 = CARTESIAN_POINT ( 'NONE',  ( 26.07500000054622902, 13.80429023900056507, 95.29460816699764791 ) ) ;
#7937 = VERTEX_POINT ( 'NONE', #398 ) ;
#7938 = DIRECTION ( 'NONE',  ( 1.000000000000000000, 0.000000000000000000, 0.000000000000000000 ) ) ;
#7939 = DIRECTION ( 'NONE',  ( 1.000000000000000000, 0.000000000000000000, 0.000000000000000000 ) ) ;
#7940 = VERTEX_POINT ( 'NONE', #7174 ) ;
#7941 = CARTESIAN_POINT ( 'NONE',  ( 6.000000000000000000, 0.000000000000000000, 0.000000000000000000 ) ) ;
#7942 = EDGE_LOOP ( 'NONE', ( #6830, #8733, #10567, #7119 ) ) ;
#7943 =( NAMED_UNIT ( * ) PLANE_ANGLE_UNIT ( ) SI_UNIT ( $, .RADIAN. ) );
#7944 = FACE_OUTER_BOUND ( 'NONE', #1350, .T. ) ;
#7945 = CARTESIAN_POINT ( 'NONE',  ( 9.483635936780883569, 16.76033569708264892, -26.34640174718215277 ) ) ;
#7946 = CARTESIAN_POINT ( 'NONE',  ( 35.57500000054622546, 26.19570976099943849, 95.29460816699764791 ) ) ;
#7947 = DIRECTION ( 'NONE',  ( 1.000000000000000000, -0.000000000000000000, -0.000000000000000000 ) ) ;
#7948 = CARTESIAN_POINT ( 'NONE',  ( -4.736720175570490632, 48.39053767382229410, -27.59648201160602454 ) ) ;
#7949 = CARTESIAN_POINT ( 'NONE',  ( 40.17500000054622689, 13.80429023900056507, 95.29460816699764791 ) ) ;
#7950 = CARTESIAN_POINT ( 'NONE',  ( 43.59999999999998721, 27.13292387221364876, 93.11078899226573924 ) ) ;
#7951 = CARTESIAN_POINT ( 'NONE',  ( 27.49999999999999645, 20.00000000000000355, 169.9999999999999716 ) ) ;
#7952 = PLANE ( 'NONE',  #5450 ) ;
#7953 = ORIENTED_EDGE ( 'NONE', *, *, #4175, .T. ) ;
#7954 = CARTESIAN_POINT ( 'NONE',  ( 33.25000000109245946, 27.13292387221364876, 93.11078899226573924 ) ) ;
#7955 = CARTESIAN_POINT ( 'NONE',  ( 1.614286760591197245, 45.25655306502918762, -24.94965407877490549 ) ) ;
#7956 = ORIENTED_EDGE ( 'NONE', *, *, #5145, .T. ) ;
#7957 = VERTEX_POINT ( 'NONE', #3368 ) ;
#7958 = CARTESIAN_POINT ( 'NONE',  ( 25.55000000109246372, 22.43689772174679575, 98.29316153445363113 ) ) ;
#7959 = DIRECTION ( 'NONE',  ( -1.000000000000000000, -0.000000000000000000, -0.000000000000000000 ) ) ;
#7960 = FACE_OUTER_BOUND ( 'NONE', #3763, .T. ) ;
#7961 = CARTESIAN_POINT ( 'NONE',  ( 33.07500000054623257, 26.19570976099943493, 86.29171490190961435 ) ) ;
#7962 = CARTESIAN_POINT ( 'NONE',  ( 31.07500000054622546, 24.28113015263587471, 84.90069139318163138 ) ) ;
#7963 = CIRCLE ( 'NONE', #5135, 0.5999999999999998668 ) ;
#7964 = CARTESIAN_POINT ( 'NONE',  ( -3.050683747432114679, 53.97481441654883838, 27.83463951904226974 ) ) ;
#7965 = CARTESIAN_POINT ( 'NONE',  ( -8.646677694484681709, 25.03392565432033479, 19.13801979030388267 ) ) ;
#7966 = CARTESIAN_POINT ( 'NONE',  ( -28.50000000000001066, 77.00000000000000000, 104.8533255156881836 ) ) ;
#7967 = ORIENTED_EDGE ( 'NONE', *, *, #1627, .F. ) ;
#7968 = CARTESIAN_POINT ( 'NONE',  ( 49.07500000054622546, 24.28113015263587471, 84.90069139318163138 ) ) ;
#7969 = CARTESIAN_POINT ( 'NONE',  ( 4.840263798742708623, 51.29555919482307758, -24.52704763417973410 ) ) ;
#7970 = DIRECTION ( 'NONE',  ( 0.000000000000000000, 0.000000000000000000, 1.000000000000000000 ) ) ;
#7971 = EDGE_LOOP ( 'NONE', ( #11116, #10735, #8923, #9671 ) ) ;
#7972 = ORIENTED_EDGE ( 'NONE', *, *, #2500, .F. ) ;
#7973 = EDGE_CURVE ( 'NONE', #2695, #11970, #9090, .T. ) ;
#7974 = DIRECTION ( 'NONE',  ( -1.000000000000000000, -0.000000000000000000, -0.000000000000000000 ) ) ;
#7975 = LINE ( 'NONE', #488, #11332 ) ;
#7976 = UNCERTAINTY_MEASURE_WITH_UNIT (LENGTH_MEASURE( 1.000000000000000082E-05 ), #11878, 'distance_accuracy_value', 'NONE');
#7977 = VECTOR ( 'NONE', #11338, 1000.000000000000000 ) ;
#7978 = DIRECTION ( 'NONE',  ( -1.000000000000000000, 0.000000000000000000, 0.000000000000000000 ) ) ;
#7979 = CARTESIAN_POINT ( 'NONE',  ( 2.912936886510098855, 54.06713064528141643, 24.83009325023465763 ) ) ;
#7980 = CARTESIAN_POINT ( 'NONE',  ( 6.910910677945284242, 27.22845955987902045, 92.80827258204288910 ) ) ;
#7981 = CARTESIAN_POINT ( 'NONE',  ( 4.337692624494786209, 47.49191884430658206, -24.62149689268095187 ) ) ;
#7982 = AXIS2_PLACEMENT_3D ( 'NONE', #7203, #9372, #5377 ) ;
#7983 = CARTESIAN_POINT ( 'NONE',  ( -2.217037138455994150, 45.50647851044359982, -24.90334479454202921 ) ) ;
#7984 = CARTESIAN_POINT ( 'NONE',  ( -2.000000000000015543, 20.00000000000000355, 90.79316153445363113 ) ) ;
#7985 = CARTESIAN_POINT ( 'NONE',  ( 0.6704130607590332858, 30.00000000000001421, -21.00000000000000355 ) ) ;
#7986 = AXIS2_PLACEMENT_3D ( 'NONE', #7825, #9669, #10090 ) ;
#7987 = CARTESIAN_POINT ( 'NONE',  ( 42.27500000054622831, 12.34168156654572535, 90.79316153445363113 ) ) ;
#7988 =( GEOMETRIC_REPRESENTATION_CONTEXT ( 3 ) GLOBAL_UNCERTAINTY_ASSIGNED_CONTEXT ( ( #11828 ) ) GLOBAL_UNIT_ASSIGNED_CONTEXT ( ( #4691, #3672, #9395 ) ) REPRESENTATION_CONTEXT ( 'NONE', 'WORKASPACE' ) );
#7989 = CARTESIAN_POINT ( 'NONE',  ( -3.050580840359966128, 46.02510565206127779, -24.81467268664276560 ) ) ;
#7990 = EDGE_LOOP ( 'NONE', ( #7185, #5811, #7449, #1052 ) ) ;
#7991 = CARTESIAN_POINT ( 'NONE',  ( -6.111033161645041289, 12.05791699719159915, -27.33052924945952356 ) ) ;
#7992 = EDGE_CURVE ( 'NONE', #10300, #6066, #11051, .T. ) ;
#7993 = CARTESIAN_POINT ( 'NONE',  ( 22.07500000054622191, 15.71886984736413417, 96.68563167572563088 ) ) ;
#7994 = CARTESIAN_POINT ( 'NONE',  ( 45.37500000054622973, 27.65831843345427998, 90.79316153445363113 ) ) ;
#7995 = CARTESIAN_POINT ( 'NONE',  ( 36.37500000054622973, 13.07298590277314432, 88.54243821818161564 ) ) ;
#7996 = CARTESIAN_POINT ( 'NONE',  ( 21.27500000054622475, 26.92701409722686634, 88.54243821818162985 ) ) ;
#7997 = CARTESIAN_POINT ( 'NONE',  ( 25.89999999999999147, 22.43689772174679575, 98.29316153445363113 ) ) ;
#7998 = DIRECTION ( 'NONE',  ( 0.000000000000000000, -0.8660254037844395958, -0.4999999999999985012 ) ) ;
#7999 = CARTESIAN_POINT ( 'NONE',  ( 29.27500000054622831, 27.65831843345427998, 90.79316153445363113 ) ) ;
#8000 = EDGE_LOOP ( 'NONE', ( #8901, #7105, #3501 ) ) ;
#8001 = CARTESIAN_POINT ( 'NONE',  ( 33.45000000109246940, 24.40838939219354842, 96.86078899226572503 ) ) ;
#8002 = VERTEX_POINT ( 'NONE', #7238 ) ;
#8003 = ORIENTED_EDGE ( 'NONE', *, *, #8455, .T. ) ;
#8004 = CONICAL_SURFACE ( 'NONE', #8402, 4.171999999999999709, 0.7853981633974609355 ) ;
#8005 = CARTESIAN_POINT ( 'NONE',  ( 1.613904720388662728, 54.74356075780413988, 27.95507540029298710 ) ) ;
#8006 = VERTEX_POINT ( 'NONE', #11111 ) ;
#8007 = CARTESIAN_POINT ( 'NONE',  ( -2.220795175011430533, 54.49171124227147089, -24.90301599942658228 ) ) ;
#8008 = CARTESIAN_POINT ( 'NONE',  ( 40.37500000054620131, 12.34168156654572357, 90.79316153445363113 ) ) ;
#8009 = CARTESIAN_POINT ( 'NONE',  ( 11.99999999999999645, 0.000000000000000000, 0.000000000000000000 ) ) ;
#8010 = CARTESIAN_POINT ( 'NONE',  ( -3.052500473972970418, 46.02637407260866809, -27.83446103405789884 ) ) ;
#8011 = CARTESIAN_POINT ( 'NONE',  ( 38.87500000054622262, 20.00000000000000355, 83.50966788445364841 ) ) ;
#8012 = CARTESIAN_POINT ( 'NONE',  ( 44.19999999999998863, 15.59161060780645691, 96.86078899226572503 ) ) ;
#8013 = VECTOR ( 'NONE', #5889, 1000.000000000000000 ) ;
#8014 = ADVANCED_FACE ( 'NONE', ( #520 ), #4381, .T. ) ;
#8015 = CARTESIAN_POINT ( 'NONE',  ( 45.37500000054622973, 26.92701409722686634, 93.04388485072563242 ) ) ;
#8016 = ORIENTED_EDGE ( 'NONE', *, *, #7265, .T. ) ;
#8017 = CARTESIAN_POINT ( 'NONE',  ( 25.35000000109246443, 26.37988106264029398, 95.42841645007781892 ) ) ;
#8018 = CARTESIAN_POINT ( 'NONE',  ( 0.6521974589784806930, 45.03172573485493047, -24.99359419162020757 ) ) ;
#8019 = ORIENTED_EDGE ( 'NONE', *, *, #7204, .F. ) ;
#8020 = CARTESIAN_POINT ( 'NONE',  ( 4.840015692395701841, 51.29662771565712376, -20.43473901115169156 ) ) ;
#8021 = ORIENTED_EDGE ( 'NONE', *, *, #3620, .F. ) ;
#8022 = DIRECTION ( 'NONE',  ( 1.000000000000000000, -0.000000000000000000, -0.000000000000000000 ) ) ;
#8023 = PRODUCT_DEFINITION_SHAPE ( 'NONE', 'NONE',  #5279 ) ;
#8024 = AXIS2_PLACEMENT_3D ( 'NONE', #11588, #8730, #1000 ) ;
#8025 = CARTESIAN_POINT ( 'NONE',  ( -3.050747483057216769, 53.97487283205587261, -24.81466456749452831 ) ) ;
#8026 = CARTESIAN_POINT ( 'NONE',  ( -50.00000000000001421, 18.00000000000000355, 188.4007504869563263 ) ) ;
#8027 = PRODUCT_DEFINITION_CONTEXT ( 'detailed design', #4973, 'design' ) ;
#8028 = CARTESIAN_POINT ( 'NONE',  ( 28.97500000054622760, 24.28113015263587471, 84.90069139318163138 ) ) ;
#8029 = CARTESIAN_POINT ( 'NONE',  ( 28.57500000054622191, 13.80429023900056684, 86.29171490190961435 ) ) ;
#8030 = CARTESIAN_POINT ( 'NONE',  ( -5.000000000000000000, 50.00000000000000000, 27.54995462791182348 ) ) ;
#8031 = CARTESIAN_POINT ( 'NONE',  ( -0.3305617426509971923, 30.00000000000001421, 21.00000000000000355 ) ) ;
#8032 = CARTESIAN_POINT ( 'NONE',  ( 22.45000000109246585, 15.59161060780646046, 84.72553407664153724 ) ) ;
#8033 = ORIENTED_EDGE ( 'NONE', *, *, #6303, .F. ) ;
#8034 = VECTOR ( 'NONE', #4229, 1000.000000000000000 ) ;
#8035 = CARTESIAN_POINT ( 'NONE',  ( 4.067198847596982247, 52.91284127144104588, -24.66711128229975003 ) ) ;
#8036 = ORIENTED_EDGE ( 'NONE', *, *, #10628, .T. ) ;
#8037 = DIRECTION ( 'NONE',  ( -0.000000000000000000, -0.000000000000000000, 1.000000000000000000 ) ) ;
#8038 = VERTEX_POINT ( 'NONE', #2359 ) ;
#8039 = CARTESIAN_POINT ( 'NONE',  ( -9.736206060811452900, 17.69460112315557510, -18.60676615975237880 ) ) ;
#8040 = AXIS2_PLACEMENT_3D ( 'NONE', #10379, #3595, #3351 ) ;
#8041 =( BOUNDED_CURVE ( )  B_SPLINE_CURVE ( 3, ( #9604, #8900, #218, #4074 ),
 .UNSPECIFIED., .F., .F. ) 
 B_SPLINE_CURVE_WITH_KNOTS ( ( 4, 4 ),
 ( 4.712388980384689674, 6.283185307179585344 ),
 .UNSPECIFIED. ) 
 CURVE ( )  GEOMETRIC_REPRESENTATION_ITEM ( )  RATIONAL_B_SPLINE_CURVE ( ( 1.000000000000000000, 0.8047378541243649375, 0.8047378541243649375, 1.000000000000000000 ) ) 
 REPRESENTATION_ITEM ( '' )  );
#8042 = CARTESIAN_POINT ( 'NONE',  ( -10.00000000000000355, 20.00000000000000355, 106.9999999999999574 ) ) ;
#8043 = EDGE_CURVE ( 'NONE', #10504, #7244, #8323, .T. ) ;
#8044 = DIRECTION ( 'NONE',  ( 1.000000000000000000, 0.000000000000000000, 0.000000000000000000 ) ) ;
#8045 = CARTESIAN_POINT ( 'NONE',  ( 6.843319662667745717, 27.29209522608180549, 92.56476529371846595 ) ) ;
#8046 = ADVANCED_FACE ( 'NONE', ( #10219 ), #11229, .F. ) ;
#8047 = CARTESIAN_POINT ( 'NONE',  ( 2.065847364689658683, 45.44381439048179772, -24.91495664786098274 ) ) ;
#8048 = CARTESIAN_POINT ( 'NONE',  ( -4.555463605440090546, 47.93247208080379806, -24.58153461361902359 ) ) ;
#8049 = DIRECTION ( 'NONE',  ( 0.000000000000000000, 0.000000000000000000, 1.000000000000000000 ) ) ;
#8050 = AXIS2_PLACEMENT_3D ( 'NONE', #7821, #7696, #8643 ) ;
#8051 = CARTESIAN_POINT ( 'NONE',  ( -3.306326722491793824, 46.23509958683961685, 27.80507441932701340 ) ) ;
#8052 = APPLICATION_CONTEXT ( 'automotive_design' ) ;
#8053 = CARTESIAN_POINT ( 'NONE',  ( 42.57500000054623257, 15.71886984736413773, 84.90069139318163138 ) ) ;
#8054 = CARTESIAN_POINT ( 'NONE',  ( -5.000000000000000888, 49.67303160952345564, -24.49489742783178059 ) ) ;
#8055 = ORIENTED_EDGE ( 'NONE', *, *, #4865, .T. ) ;
#8056 = ADVANCED_FACE ( 'NONE', ( #9027 ), #3436, .F. ) ;
#8057 = CARTESIAN_POINT ( 'NONE',  ( -1.297965663867492347, 54.83959394270241461, 24.96833505342767978 ) ) ;
#8058 = CARTESIAN_POINT ( 'NONE',  ( 22.27500000054622120, 13.07298590277314254, 93.04388485072563242 ) ) ;
#8059 = CARTESIAN_POINT ( 'NONE',  ( 47.47500000054622404, 26.92701409722686634, 93.04388485072563242 ) ) ;
#8060 = CARTESIAN_POINT ( 'NONE',  ( 34.77500000054622831, 20.00000000000000355, 83.50966788445364841 ) ) ;
#8061 = CARTESIAN_POINT ( 'NONE',  ( 22.67500000054622333, 15.71886984736413773, 84.90069139318163138 ) ) ;
#8062 = CARTESIAN_POINT ( 'NONE',  ( 6.000000000000000000, 2.919948986426526005, -5.057500000000003659 ) ) ;
#8063 = FILL_AREA_STYLE_COLOUR ( '', #11735 ) ;
#8064 = CARTESIAN_POINT ( 'NONE',  ( 23.87500000054622973, 17.63344945572769973, 98.07665518445361386 ) ) ;
#8065 = ORIENTED_EDGE ( 'NONE', *, *, #10383, .F. ) ;
#8066 = ADVANCED_FACE ( 'NONE', ( #2416 ), #2297, .T. ) ;
#8067 = CARTESIAN_POINT ( 'NONE',  ( 12.59999999999999964, 0.000000000000000000, 0.000000000000000000 ) ) ;
#8068 = ORIENTED_EDGE ( 'NONE', *, *, #5111, .T. ) ;
#8069 = AXIS2_PLACEMENT_3D ( 'NONE', #11810, #4900, #9663 ) ;
#8070 = ORIENTED_EDGE ( 'NONE', *, *, #5608, .F. ) ;
#8071 = ORIENTED_EDGE ( 'NONE', *, *, #6421, .T. ) ;
#8072 = CARTESIAN_POINT ( 'NONE',  ( -4.743369866101525112, 51.61445767325203349, -24.54621253249761637 ) ) ;
#8073 = EDGE_CURVE ( 'NONE', #2265, #438, #8198, .T. ) ;
#8074 = CIRCLE ( 'NONE', #8878, 5.035999999999999588 ) ;
#8075 = CARTESIAN_POINT ( 'NONE',  ( 37.37500000054622262, 27.65831843345427998, 90.79316153445363113 ) ) ;
#8076 = DIRECTION ( 'NONE',  ( -1.000000000000000000, -0.000000000000000000, -0.000000000000000000 ) ) ;
#8077 = CARTESIAN_POINT ( 'NONE',  ( -27.49999999999999645, 12.50000000000001066, 145.0000000000000000 ) ) ;
#8078 = CARTESIAN_POINT ( 'NONE',  ( 39.67500000054622689, 24.28113015263587116, 96.68563167572563088 ) ) ;
#8079 = CARTESIAN_POINT ( 'NONE',  ( 40.49999999999999289, 12.11403331821300533, 90.79316153445363113 ) ) ;
#8080 = CARTESIAN_POINT ( 'NONE',  ( 44.27500000054622120, 12.34168156654572535, 90.79316153445363113 ) ) ;
#8081 = EDGE_LOOP ( 'NONE', ( #296, #6255 ) ) ;
#8082 = CARTESIAN_POINT ( 'NONE',  ( 22.75000000109246656, 22.43689772174679575, 83.29316153445363113 ) ) ;
#8083 = DIRECTION ( 'NONE',  ( 0.000000000000000000, 0.000000000000000000, 1.000000000000000000 ) ) ;
#8084 = ORIENTED_EDGE ( 'NONE', *, *, #7903, .F. ) ;
#8085 = AXIS2_PLACEMENT_3D ( 'NONE', #8679, #2718, #5580 ) ;
#8086 = CARTESIAN_POINT ( 'NONE',  ( -6.102022788481106907, 27.92916547445571140, 27.32823034940942364 ) ) ;
#8087 = ORIENTED_EDGE ( 'NONE', *, *, #9543, .T. ) ;
#8088 = CARTESIAN_POINT ( 'NONE',  ( 6.115126465005007006, 12.06069949568701283, 27.32969027731172673 ) ) ;
#8089 = EDGE_CURVE ( 'NONE', #1348, #6557, #2619, .T. ) ;
#8090 = CARTESIAN_POINT ( 'NONE',  ( 41.05000000109246372, 27.13292387221364876, 88.47553407664153724 ) ) ;
#8091 = FACE_OUTER_BOUND ( 'NONE', #7468, .T. ) ;
#8092 = CARTESIAN_POINT ( 'NONE',  ( 32.47500000054623825, 13.80429023900056684, 86.29171490190961435 ) ) ;
#8093 = CARTESIAN_POINT ( 'NONE',  ( 34.27500000054622120, 13.07298590277314254, 93.04388485072563242 ) ) ;
#8094 = CYLINDRICAL_SURFACE ( 'NONE', #10019, 7.499999999999978684 ) ;
#8095 = EDGE_CURVE ( 'NONE', #8953, #3460, #5935, .T. ) ;
#8096 = CLOSED_SHELL ( 'NONE', ( #3533, #6334, #7744, #615, #6832, #9561, #8922, #5518, #6293, #2886, #6947, #411, #7077, #11693, #6144, #10653, #212, #9316, #7738, #9259, #639, #372, #3953, #3556, #1649, #713, #3579, #4496, #3165, #1828, #7913, #9492, #6638, #5464, #6200, #12465, #2818, #11699, #1146, #6267, #11385, #6290, #7283, #10488, #7852, #7614, #857, #1547, #11261, #8770, #9950, #2638, #8582, #12022, #10557, #3432, #365, #1920, #8475, #7833, #12238, #756, #12419, #9960, #4963, #9185, #2607, #3472, #6765, #10253, #4108, #9454, #1252, #1898, #7523, #4649, #4245, #2255, #7781, #7932, #2738, #6531, #6739, #4441, #8537, #6903, #11882, #11343, #11291, #8377, #5117, #7032 ) ) ;
#8097 = CARTESIAN_POINT ( 'NONE',  ( 0.000000000000000000, -2.342598717236902051, 4.057500000000004547 ) ) ;
#8098 = ORIENTED_EDGE ( 'NONE', *, *, #8738, .T. ) ;
#8099 = CARTESIAN_POINT ( 'NONE',  ( 40.95000000109246940, 26.37988106264029398, 86.15790661882942914 ) ) ;
#8100 = ORIENTED_EDGE ( 'NONE', *, *, #561, .F. ) ;
#8101 = CARTESIAN_POINT ( 'NONE',  ( 6.000000000000000000, 2.919948986426539772, 5.057499999999996554 ) ) ;
#8102 = ORIENTED_EDGE ( 'NONE', *, *, #5440, .F. ) ;
#8103 = CARTESIAN_POINT ( 'NONE',  ( -8.968054450094975039, 15.52726727364191994, -18.99089028591819428 ) ) ;
#8104 = CARTESIAN_POINT ( 'NONE',  ( 4.153883524164314167, 10.89765663934413276, -24.65439000785841372 ) ) ;
#8105 = AXIS2_PLACEMENT_3D ( 'NONE', #9355, #7440, #7251 ) ;
#8106 = DIRECTION ( 'NONE',  ( 0.000000000000000000, 1.000000000000000000, -1.039664082171044875E-15 ) ) ;
#8107 = DIRECTION ( 'NONE',  ( 0.000000000000000000, 0.000000000000000000, -1.000000000000000000 ) ) ;
#8108 = CARTESIAN_POINT ( 'NONE',  ( 37.85000000109246798, 15.59161060780645691, 96.86078899226572503 ) ) ;
#8109 = CIRCLE ( 'NONE', #6090, 7.500000000000000000 ) ;
#8110 = CARTESIAN_POINT ( 'NONE',  ( 4.164372531543180322, 29.09754760689071063, 20.58525091202328738 ) ) ;
#8111 = LINE ( 'NONE', #5320, #3101 ) ;
#8112 = CARTESIAN_POINT ( 'NONE',  ( 12.59999999999999964, 8.082668874372531019E-16, 6.599999999999999645 ) ) ;
#8113 = CARTESIAN_POINT ( 'NONE',  ( 5.000000000000000000, 50.00000000000000000, -28.00000000000000711 ) ) ;
#8114 = EDGE_LOOP ( 'NONE', ( #1738, #5210 ) ) ;
#8115 =( BOUNDED_CURVE ( )  B_SPLINE_CURVE ( 2, ( #3965, #2890, #8981, #10618, #4090, #10809, #4859, #3141, #1931, #7012, #5053 ),
 .UNSPECIFIED., .F., .F. ) 
 B_SPLINE_CURVE_WITH_KNOTS ( ( 3, 2, 2, 2, 2, 3 ),
 ( 0.5000000000000000000, 0.5066666666666667096, 0.5133333333333333082, 0.5200000000000000178, 0.5266666666666666163, 0.5333333333333333259 ),
 .UNSPECIFIED. ) 
 CURVE ( )  GEOMETRIC_REPRESENTATION_ITEM ( )  RATIONAL_B_SPLINE_CURVE ( ( 1.000000000000000000, 0.9510565162951535312, 1.000000000000000000, 0.9510565162951535312, 1.000000000000000000, 0.9510565162951535312, 1.000000000000000000, 0.9510565162951535312, 1.000000000000000000, 0.9510565162951535312, 1.000000000000000000 ) ) 
 REPRESENTATION_ITEM ( '' )  );
#8116 = CARTESIAN_POINT ( 'NONE',  ( 6.999999999999978684, 20.00000000000000355, 109.9999999999999858 ) ) ;
#8117 = EDGE_CURVE ( 'NONE', #574, #1317, #10692, .T. ) ;
#8118 = CARTESIAN_POINT ( 'NONE',  ( 5.000000000000000000, 50.33107439471904598, 24.49489742783178770 ) ) ;
#8119 = CARTESIAN_POINT ( 'NONE',  ( 44.17500000054622689, 13.80429023900056507, 95.29460816699764791 ) ) ;
#8120 = CARTESIAN_POINT ( 'NONE',  ( 35.27500000054621410, 27.65831843345427998, 90.79316153445363113 ) ) ;
#8121 = CARTESIAN_POINT ( 'NONE',  ( 8.669261784762754885, 15.00032884213714546, 96.40336117293375651 ) ) ;
#8122 = CARTESIAN_POINT ( 'NONE',  ( 20.09999999999998366, 17.56310227825320425, 98.29316153445363113 ) ) ;
#8123 = CARTESIAN_POINT ( 'NONE',  ( 49.89999999999998437, 22.43689772174679575, 98.29316153445363113 ) ) ;
#8124 = CARTESIAN_POINT ( 'NONE',  ( 26.77500000054622831, 20.00000000000000355, 83.50966788445364841 ) ) ;
#8125 = VERTEX_POINT ( 'NONE', #9462 ) ;
#8126 = AXIS2_PLACEMENT_3D ( 'NONE', #5466, #4623, #6405 ) ;
#8127 = PRODUCT ( 'Cast Iron Bearing Support Block', 'Cast Iron Bearing Support Block', '', ( #3986 ) ) ;
#8128 = CARTESIAN_POINT ( 'NONE',  ( 6.955575927950914131E-22, 45.00000000000000711, -25.00000000000000000 ) ) ;
#8129 = VERTEX_POINT ( 'NONE', #12249 ) ;
#8130 = ORIENTED_EDGE ( 'NONE', *, *, #3266, .T. ) ;
#8131 = CARTESIAN_POINT ( 'NONE',  ( 38.29999999999999005, 13.62011893735970958, 95.42841645007781892 ) ) ;
#8132 = ORIENTED_EDGE ( 'NONE', *, *, #9835, .T. ) ;
#8133 = EDGE_CURVE ( 'NONE', #6810, #1088, #3304, .T. ) ;
#8134 = SHAPE_REPRESENTATION_RELATIONSHIP ( 'NONE' , 'NONE' ,  #8561, #971 ) ;
#8135 = AXIS2_PLACEMENT_3D ( 'NONE', #8731, #10871, #8969 ) ;
#8136 = CARTESIAN_POINT ( 'NONE',  ( 34.77500000054621410, 17.63344945572770328, 83.50966788445364841 ) ) ;
#8137 = DIRECTION ( 'NONE',  ( -1.000000000000000000, -0.000000000000000000, -0.000000000000000000 ) ) ;
#8138 = EDGE_CURVE ( 'NONE', #10066, #5241, #11512, .T. ) ;
#8139 = CARTESIAN_POINT ( 'NONE',  ( 12.59999999999999964, 0.000000000000000000, -6.599999999999999645 ) ) ;
#8140 = CARTESIAN_POINT ( 'NONE',  ( 37.57500000054623257, 26.19570976099943493, 95.29460816699764791 ) ) ;
#8141 = CARTESIAN_POINT ( 'NONE',  ( 38.59999999999998721, 12.86707612778636012, 88.47553407664152303 ) ) ;
#8142 = CARTESIAN_POINT ( 'NONE',  ( 43.37500000054622973, 26.92701409722686634, 93.04388485072563242 ) ) ;
#8143 = ORIENTED_EDGE ( 'NONE', *, *, #2280, .F. ) ;
#8144 = CARTESIAN_POINT ( 'NONE',  ( 27.55000000109246017, 22.43689772174679575, 98.29316153445363113 ) ) ;
#8145 = CARTESIAN_POINT ( 'NONE',  ( 0.000000000000000000, 5.839897972853064445, -8.673617379884035472E-15 ) ) ;
#8146 = ORIENTED_EDGE ( 'NONE', *, *, #6966, .F. ) ;
#8147 = EDGE_CURVE ( 'NONE', #8255, #188, #8565, .T. ) ;
#8148 = DIRECTION ( 'NONE',  ( 0.000000000000000000, 0.000000000000000000, -1.000000000000000000 ) ) ;
#8149 = EDGE_LOOP ( 'NONE', ( #1737, #6, #712, #7045 ) ) ;
#8150 = CYLINDRICAL_SURFACE ( 'NONE', #4855, 7.499999999999992895 ) ;
#8151 = CARTESIAN_POINT ( 'NONE',  ( 4.744280297632045951, 48.38773530922238564, -27.59543500301886354 ) ) ;
#8152 = CARTESIAN_POINT ( 'NONE',  ( 25.79999999999998650, 24.40838939219354842, 96.86078899226572503 ) ) ;
#8153 = EDGE_CURVE ( 'NONE', #10690, #1585, #7615, .T. ) ;
#8154 = CARTESIAN_POINT ( 'NONE',  ( 29.67500000054623044, 22.36655054427230027, 98.07665518445361386 ) ) ;
#8155 = CARTESIAN_POINT ( 'NONE',  ( 27.67500000054622333, 24.28113015263587116, 96.68563167572563088 ) ) ;
#8156 = CARTESIAN_POINT ( 'NONE',  ( -111.8465843842649292, 84.49999999999998579, 101.8533255156881978 ) ) ;
#8157 = CARTESIAN_POINT ( 'NONE',  ( 9.999999999999991118, 20.00000000000000355, 187.9999999999999716 ) ) ;
#8158 = VERTEX_POINT ( 'NONE', #9581 ) ;
#8159 = EDGE_CURVE ( 'NONE', #10297, #10983, #3552, .T. ) ;
#8160 = CARTESIAN_POINT ( 'NONE',  ( 46.75000000109246656, 22.43689772174679575, 83.29316153445363113 ) ) ;
#8161 =( NAMED_UNIT ( * ) SI_UNIT ( $, .STERADIAN. ) SOLID_ANGLE_UNIT ( ) );
#8162 = VERTEX_POINT ( 'NONE', #5591 ) ;
#8163 = CARTESIAN_POINT ( 'NONE',  ( 34.72841614740047333, 18.00000000000000355, 152.2284161474004520 ) ) ;
#8164 =( BOUNDED_CURVE ( )  B_SPLINE_CURVE ( 2, ( #6969, #3292, #6396, #11033, #7221, #7155, #9136, #9073, #5327, #7343, #9197 ),
 .UNSPECIFIED., .F., .F. ) 
 B_SPLINE_CURVE_WITH_KNOTS ( ( 3, 2, 2, 2, 2, 3 ),
 ( 0.6999999999999999556, 0.7066666666666666652, 0.7133333333333333748, 0.7199999999999999734, 0.7266666666666666829, 0.7333333333333332815 ),
 .UNSPECIFIED. ) 
 CURVE ( )  GEOMETRIC_REPRESENTATION_ITEM ( )  RATIONAL_B_SPLINE_CURVE ( ( 1.000000000000000000, 0.9510565162951535312, 1.000000000000000000, 0.9510565162951535312, 1.000000000000000000, 0.9510565162951535312, 1.000000000000000000, 0.9510565162951535312, 1.000000000000000000, 0.9510565162951535312, 1.000000000000000000 ) ) 
 REPRESENTATION_ITEM ( '' )  );
#8165 = ORIENTED_EDGE ( 'NONE', *, *, #791, .F. ) ;
#8166 = CARTESIAN_POINT ( 'NONE',  ( -2.620496854523448604, 10.32661740714168097, -24.87086379260451707 ) ) ;
#8167 = CARTESIAN_POINT ( 'NONE',  ( 6.114177788104627531, 12.06044222946883693, -24.24708634001311580 ) ) ;
#8168 = ADVANCED_FACE ( 'NONE', ( #5651 ), #11202, .F. ) ;
#8169 = DIRECTION ( 'NONE',  ( -1.000000000000000000, -0.000000000000000000, -0.000000000000000000 ) ) ;
#8170 = VECTOR ( 'NONE', #6528, 1000.000000000000000 ) ;
#8171 = DIRECTION ( 'NONE',  ( 1.000000000000000000, -0.000000000000000000, -0.000000000000000000 ) ) ;
#8172 = CARTESIAN_POINT ( 'NONE',  ( 5.000000000000000000, 50.00000000000000000, 27.54995462791182703 ) ) ;
#8173 = FACE_OUTER_BOUND ( 'NONE', #8712, .T. ) ;
#8174 = CARTESIAN_POINT ( 'NONE',  ( -9.918964982526143004, 18.68741511430571833, 26.18425748175654988 ) ) ;
#8175 = DIRECTION ( 'NONE',  ( -0.000000000000000000, -0.000000000000000000, 1.000000000000000000 ) ) ;
#8176 = TOROIDAL_SURFACE ( 'NONE', #4526, 6.500000000000000888, 1.500000000000000000 ) ;
#8177 = CARTESIAN_POINT ( 'NONE',  ( 4.742699133420079427, 48.38316774318188607, 20.45784509570819765 ) ) ;
#8178 = ORIENTED_EDGE ( 'NONE', *, *, #2963, .F. ) ;
#8179 = CARTESIAN_POINT ( 'NONE',  ( -8.127975879305816775, 14.16556116651870845, -26.79499133733385108 ) ) ;
#8180 = CARTESIAN_POINT ( 'NONE',  ( 4.743169864344128683, 48.38453593858750423, 24.54625634892152775 ) ) ;
#8181 = CARTESIAN_POINT ( 'NONE',  ( 0.000000000000000000, -5.839897972853060892, 7.806255641895631925E-15 ) ) ;
#8182 = CARTESIAN_POINT ( 'NONE',  ( 45.77500000054622120, 22.36655054427230027, 98.07665518445361386 ) ) ;
#8183 = VECTOR ( 'NONE', #414, 1000.000000000000000 ) ;
#8184 = CARTESIAN_POINT ( 'NONE',  ( 29.07500000054623257, 26.19570976099943849, 86.29171490190961435 ) ) ;
#8185 = CARTESIAN_POINT ( 'NONE',  ( 9.917674697986294419, 18.67684296126092747, -22.94866065126248600 ) ) ;
#8186 = CARTESIAN_POINT ( 'NONE',  ( 45.45000000109246230, 24.40838939219354842, 96.86078899226572503 ) ) ;
#8187 = PRODUCT_DEFINITION_FORMATION_WITH_SPECIFIED_SOURCE ( 'ANY', '', #6786, .NOT_KNOWN. ) ;
#8188 = CARTESIAN_POINT ( 'NONE',  ( 32.99999999999998579, 20.00000000000000355, 83.29316153445364534 ) ) ;
#8189 = CYLINDRICAL_SURFACE ( 'NONE', #10923, 7.499999999999992895 ) ;
#8190 = CARTESIAN_POINT ( 'NONE',  ( 29.07500000054623257, 26.19570976099943493, 86.29171490190961435 ) ) ;
#8191 = ORIENTED_EDGE ( 'NONE', *, *, #1458, .T. ) ;
#8192 = CARTESIAN_POINT ( 'NONE',  ( 33.15000000109246514, 27.88596668178699645, 90.79316153445363113 ) ) ;
#8193 = DIRECTION ( 'NONE',  ( 0.000000000000000000, 0.000000000000000000, -1.000000000000000000 ) ) ;
#8194 = ORIENTED_EDGE ( 'NONE', *, *, #1791, .F. ) ;
#8195 = AXIS2_PLACEMENT_3D ( 'NONE', #12083, #4397, #12144 ) ;
#8196 = CIRCLE ( 'NONE', #6968, 7.500000000000000000 ) ;
#8197 = CARTESIAN_POINT ( 'NONE',  ( 29.07500000054622191, 24.28113015263587471, 84.90069139318163138 ) ) ;
#8198 = LINE ( 'NONE', #11943, #1681 ) ;
#8199 = CARTESIAN_POINT ( 'NONE',  ( 48.07500000054623257, 13.80429023900056507, 95.29460816699764791 ) ) ;
#8200 = CARTESIAN_POINT ( 'NONE',  ( 33.57500000054622546, 26.19570976099943493, 95.29460816699764791 ) ) ;
#8201 = CARTESIAN_POINT ( 'NONE',  ( 36.69999999999999574, 13.62011893735971135, 86.15790661882942914 ) ) ;
#8202 = EDGE_CURVE ( 'NONE', #4145, #9642, #5739, .T. ) ;
#8203 = CARTESIAN_POINT ( 'NONE',  ( 46.07500000054623257, 13.80429023900056507, 95.29460816699764791 ) ) ;
#8204 = ORIENTED_EDGE ( 'NONE', *, *, #3967, .F. ) ;
#8205 = AXIS2_PLACEMENT_3D ( 'NONE', #5131, #11852, #5002 ) ;
#8206 = CARTESIAN_POINT ( 'NONE',  ( 26.65000000109246514, 20.00000000000000355, 83.29316153445364534 ) ) ;
#8207 = CARTESIAN_POINT ( 'NONE',  ( -8.658175568303594360, 14.98574592473889311, 23.45342671841680371 ) ) ;
#8208 = VERTEX_POINT ( 'NONE', #9397 ) ;
#8209 = CARTESIAN_POINT ( 'NONE',  ( 27.49999999999999645, 20.00000000000000355, 169.9999999999999716 ) ) ;
#8210 = ORIENTED_EDGE ( 'NONE', *, *, #5907, .T. ) ;
#8211 = CARTESIAN_POINT ( 'NONE',  ( 3.061616997868383043E-15, 0.000000000000000000, 25.00000000000000000 ) ) ;
#8212 = PLANE ( 'NONE',  #10936 ) ;
#8213 = CARTESIAN_POINT ( 'NONE',  ( 36.55000000109246372, 17.56310227825317583, 83.29316153445365956 ) ) ;
#8214 = CIRCLE ( 'NONE', #7601, 10.00000000000000888 ) ;
#8215 = DIRECTION ( 'NONE',  ( -1.000000000000000000, 0.000000000000000000, 0.000000000000000000 ) ) ;
#8216 = CARTESIAN_POINT ( 'NONE',  ( 23.07500000054622902, 26.19570976099943493, 86.29171490190961435 ) ) ;
#8217 = CARTESIAN_POINT ( 'NONE',  ( 26.67500000054622333, 15.71886984736413773, 84.90069139318163138 ) ) ;
#8218 = APPLICATION_CONTEXT ( 'automotive_design' ) ;
#8219 = DIRECTION ( 'NONE',  ( 1.000000000000000000, 0.000000000000000000, 0.000000000000000000 ) ) ;
#8220 = CARTESIAN_POINT ( 'NONE',  ( 0.000000000000000000, 2.919948986426526005, -5.057500000000003659 ) ) ;
#8221 = ORIENTED_EDGE ( 'NONE', *, *, #6023, .T. ) ;
#8222 = CARTESIAN_POINT ( 'NONE',  ( 43.05000000109246372, 27.13292387221364876, 88.47553407664153724 ) ) ;
#8223 = ORIENTED_EDGE ( 'NONE', *, *, #2784, .T. ) ;
#8224 = LINE ( 'NONE', #2565, #9250 ) ;
#8225 = EDGE_CURVE ( 'NONE', #9848, #2831, #7677, .T. ) ;
#8226 = ORIENTED_EDGE ( 'NONE', *, *, #11408, .F. ) ;
#8227 = CARTESIAN_POINT ( 'NONE',  ( 5.000000000000000000, 50.33148762970345302, 20.39607805437114507 ) ) ;
#8228 = CARTESIAN_POINT ( 'NONE',  ( 9.482520708152488709, 16.75818430496380529, -23.13341755400983502 ) ) ;
#8229 = CARTESIAN_POINT ( 'NONE',  ( -31.74999999999995737, 0.000000000000000000, 0.000000000000000000 ) ) ;
#8230 = CIRCLE ( 'NONE', #2753, 23.49999999999999289 ) ;
#8231 = CARTESIAN_POINT ( 'NONE',  ( 3.419345135684301873, 53.65163791593241172, 24.76532955609361863 ) ) ;
#8232 = AXIS2_PLACEMENT_3D ( 'NONE', #6948, #5058, #8920 ) ;
#8233 = CARTESIAN_POINT ( 'NONE',  ( -5.038456156925416707, 11.33776630238819116, 24.49323865847078707 ) ) ;
#8234 = CARTESIAN_POINT ( 'NONE',  ( 22.89999999999998792, 17.56310227825320425, 83.29316153445363113 ) ) ;
#8235 = SHAPE_REPRESENTATION ( 'Support Axle', ( #9021 ), #3536 ) ;
#8236 = CARTESIAN_POINT ( 'NONE',  ( -3.255256241227468372, 10.53893016368868096, 20.74860095102915736 ) ) ;
#8237 = CARTESIAN_POINT ( 'NONE',  ( 24.99999999999998579, 20.00000000000000355, 83.29316153445364534 ) ) ;
#8238 = LINE ( 'NONE', #7276, #10243 ) ;
#8239 = EDGE_CURVE ( 'NONE', #12263, #7138, #336, .T. ) ;
#8240 = CARTESIAN_POINT ( 'NONE',  ( -3.974640651900942512, 46.94910328357455143, -24.68270373814292640 ) ) ;
#8241 = ORIENTED_EDGE ( 'NONE', *, *, #2784, .F. ) ;
#8242 = CARTESIAN_POINT ( 'NONE',  ( -50.00000000000001421, 0.000000000000000000, 169.9999999999999716 ) ) ;
#8243 = EDGE_CURVE ( 'NONE', #6932, #9559, #8441, .T. ) ;
#8244 = DIRECTION ( 'NONE',  ( 0.000000000000000000, 1.000000000000000000, 0.000000000000000000 ) ) ;
#8245 = CARTESIAN_POINT ( 'NONE',  ( 47.27500000054622831, 26.92701409722686634, 88.54243821818162985 ) ) ;
#8246 = AXIS2_PLACEMENT_3D ( 'NONE', #10259, #625, #1634 ) ;
#8247 = CARTESIAN_POINT ( 'NONE',  ( 25.77500000054622831, 20.00000000000000355, 98.07665518445361386 ) ) ;
#8248 = CARTESIAN_POINT ( 'NONE',  ( 9.673501139021151829, 17.38172013086462542, -23.05305332146628317 ) ) ;
#8249 = CARTESIAN_POINT ( 'NONE',  ( -50.00000000000001421, 22.00000000000000000, 152.2284161474004520 ) ) ;
#8250 = CARTESIAN_POINT ( 'NONE',  ( 40.09999999999998721, 17.56310227825322556, 98.29316153445364534 ) ) ;
#8251 = CARTESIAN_POINT ( 'NONE',  ( -50.00000000000001421, 20.00000000000000000, 145.0000000000000000 ) ) ;
#8252 = EDGE_CURVE ( 'NONE', #3301, #7750, #1623, .T. ) ;
#8253 = ORIENTED_EDGE ( 'NONE', *, *, #7470, .T. ) ;
#8254 = CARTESIAN_POINT ( 'NONE',  ( 6.000000000000000000, 5.839897972853064445, -8.673617379884035472E-15 ) ) ;
#8255 = VERTEX_POINT ( 'NONE', #5776 ) ;
#8256 = VECTOR ( 'NONE', #3946, 1000.000000000000114 ) ;
#8257 = CARTESIAN_POINT ( 'NONE',  ( 29.37500000054622618, 27.65831843345427998, 90.79316153445363113 ) ) ;
#8258 = CARTESIAN_POINT ( 'NONE',  ( -31.74999999999995737, 0.000000000000000000, 0.000000000000000000 ) ) ;
#8259 = CARTESIAN_POINT ( 'NONE',  ( 44.67500000054622689, 17.63344945572770328, 83.50966788445364841 ) ) ;
#8260 = CARTESIAN_POINT ( 'NONE',  ( 34.27500000054622120, 13.07298590277314254, 93.04388485072563242 ) ) ;
#8261 = CARTESIAN_POINT ( 'NONE',  ( 34.89999999999997726, 17.56310227825321135, 83.29316153445363113 ) ) ;
#8262 = AXIS2_PLACEMENT_3D ( 'NONE', #10429, #1802, #6747 ) ;
#8263 = LINE ( 'NONE', #4, #3621 ) ;
#8264 = CARTESIAN_POINT ( 'NONE',  ( 43.27500000054623541, 27.65831843345427998, 90.79316153445363113 ) ) ;
#8265 = ORIENTED_EDGE ( 'NONE', *, *, #6076, .F. ) ;
#8266 = CARTESIAN_POINT ( 'NONE',  ( 24.45000000109246585, 15.59161060780646046, 84.72553407664153724 ) ) ;
#8267 = CARTESIAN_POINT ( 'NONE',  ( -4.336726535208759614, 47.49029485220934532, 24.62166619875052831 ) ) ;
#8268 = ORIENTED_EDGE ( 'NONE', *, *, #4049, .F. ) ;
#8269 = PLANE ( 'NONE',  #7726 ) ;
#8270 = ORIENTED_EDGE ( 'NONE', *, *, #11892, .T. ) ;
#8271 = LINE ( 'NONE', #10175, #2524 ) ;
#8272 = CIRCLE ( 'NONE', #7459, 7.499999999999978684 ) ;
#8273 = CARTESIAN_POINT ( 'NONE',  ( 21.55000000109246372, 22.43689772174679575, 98.29316153445363113 ) ) ;
#8274 = CARTESIAN_POINT ( 'NONE',  ( 12.59999999999999964, 0.000000000000000000, 6.000000000000003553 ) ) ;
#8275 = ADVANCED_FACE ( 'NONE', ( #11794 ), #194, .F. ) ;
#8276 = CARTESIAN_POINT ( 'NONE',  ( 0.000000000000000000, -3.000000000000003109, 0.000000000000000000 ) ) ;
#8277 = CARTESIAN_POINT ( 'NONE',  ( 23.37500000054622973, 26.92701409722686634, 93.04388485072563242 ) ) ;
#8278 = CARTESIAN_POINT ( 'NONE',  ( 22.67500000054622333, 15.71886984736413773, 84.90069139318163138 ) ) ;
#8279 = CARTESIAN_POINT ( 'NONE',  ( 7.515035695928145465, 26.60532803001909841, 26.97351675661644421 ) ) ;
#8280 = CARTESIAN_POINT ( 'NONE',  ( 10.00000000000000000, 6.613092715395708453E-16, 5.400000000000001243 ) ) ;
#8281 = CIRCLE ( 'NONE', #1589, 6.600000000000003197 ) ;
#8282 = ORIENTED_EDGE ( 'NONE', *, *, #12537, .T. ) ;
#8283 = CARTESIAN_POINT ( 'NONE',  ( 42.05000000109246372, 12.86707612778636012, 93.11078899226572503 ) ) ;
#8284 = CARTESIAN_POINT ( 'NONE',  ( 4.067198847596982247, 52.91284127144104588, -24.66711128229975003 ) ) ;
#8285 = ORIENTED_EDGE ( 'NONE', *, *, #8470, .F. ) ;
#8286 = CARTESIAN_POINT ( 'NONE',  ( 30.15000000109246159, 12.11403331821300533, 90.79316153445363113 ) ) ;
#8287 = VERTEX_POINT ( 'NONE', #4824 ) ;
#8288 = CARTESIAN_POINT ( 'NONE',  ( -9.868061339005878452, 18.34793401400264301, -22.97011835729309936 ) ) ;
#8289 = CARTESIAN_POINT ( 'NONE',  ( 7.946724766127979400, 13.89530605390606688, -23.70643652970303350 ) ) ;
#8290 =( GEOMETRIC_REPRESENTATION_CONTEXT ( 3 ) GLOBAL_UNCERTAINTY_ASSIGNED_CONTEXT ( ( #12538 ) ) GLOBAL_UNIT_ASSIGNED_CONTEXT ( ( #11679, #3738, #7683 ) ) REPRESENTATION_CONTEXT ( 'NONE', 'WORKASPACE' ) );
#8291 = CARTESIAN_POINT ( 'NONE',  ( 29.99999999999998934, 20.00000000000000355, 98.29316153445363113 ) ) ;
#8292 = VECTOR ( 'NONE', #2382, 1000.000000000000000 ) ;
#8293 = CARTESIAN_POINT ( 'NONE',  ( 0.000000000000000000, 0.000000000000000000, 109.9999999999999858 ) ) ;
#8294 = EDGE_CURVE ( 'NONE', #7244, #3052, #7762, .T. ) ;
#8295 = CARTESIAN_POINT ( 'NONE',  ( -9.983814731900727324, 19.34254964819328038, 22.91996290304706108 ) ) ;
#8296 = DIRECTION ( 'NONE',  ( 0.000000000000000000, 0.000000000000000000, -1.000000000000000000 ) ) ;
#8297 = CARTESIAN_POINT ( 'NONE',  ( 42.19999999999998863, 15.59161060780645691, 96.86078899226572503 ) ) ;
#8298 = CARTESIAN_POINT ( 'NONE',  ( 6.000000000000000000, 4.379923479639802331, 2.528749999999992948 ) ) ;
#8299 = CARTESIAN_POINT ( 'NONE',  ( 10.00000000000000355, 20.00000000000000355, 22.91287847477919826 ) ) ;
#8300 = VECTOR ( 'NONE', #9142, 1000.000000000000000 ) ;
#8301 = EDGE_CURVE ( 'NONE', #188, #8255, #8978, .T. ) ;
#8302 = CARTESIAN_POINT ( 'NONE',  ( 23.69999999999998508, 26.37988106264029398, 95.42841645007781892 ) ) ;
#8303 = ORIENTED_EDGE ( 'NONE', *, *, #6998, .T. ) ;
#8304 = AXIS2_PLACEMENT_3D ( 'NONE', #2745, #11494, #6603 ) ;
#8305 = CARTESIAN_POINT ( 'NONE',  ( 4.338021161404794768, 47.49236434914906368, 24.62144314154611990 ) ) ;
#8306 = CARTESIAN_POINT ( 'NONE',  ( 3.419345135684301873, 53.65163791593241172, 24.76532955609361863 ) ) ;
#8307 = CARTESIAN_POINT ( 'NONE',  ( 39.17500000054621978, 26.19570976099943493, 86.29171490190961435 ) ) ;
#8308 = CARTESIAN_POINT ( 'NONE',  ( 26.67500000054622689, 17.63344945572770328, 83.50966788445364841 ) ) ;
#8309 = CARTESIAN_POINT ( 'NONE',  ( 6.843143145516298098, 12.70774044341717968, 89.02228661475956528 ) ) ;
#8310 = DIRECTION ( 'NONE',  ( 1.000000000000000000, 0.000000000000000000, 0.000000000000000000 ) ) ;
#8311 = LINE ( 'NONE', #4497, #4945 ) ;
#8312 = CARTESIAN_POINT ( 'NONE',  ( 5.000000000000000000, 4.685197434473814759, -5.637851296924623057E-15 ) ) ;
#8313 = ORIENTED_EDGE ( 'NONE', *, *, #6049, .T. ) ;
#8314 = EDGE_CURVE ( 'NONE', #7136, #938, #3502, .T. ) ;
#8315 = DIRECTION ( 'NONE',  ( 1.000000000000000000, -0.000000000000000000, -0.000000000000000000 ) ) ;
#8316 = ORIENTED_EDGE ( 'NONE', *, *, #1196, .F. ) ;
#8317 = AXIS2_PLACEMENT_3D ( 'NONE', #9862, #6742, #156 ) ;
#8318 = CARTESIAN_POINT ( 'NONE',  ( 0.000000000000000000, 67.00000000000000000, 0.000000000000000000 ) ) ;
#8319 = DIRECTION ( 'NONE',  ( 1.000000000000000000, 0.000000000000000000, 0.000000000000000000 ) ) ;
#8320 = EDGE_CURVE ( 'NONE', #6932, #409, #2488, .T. ) ;
#8321 = EDGE_CURVE ( 'NONE', #10286, #6911, #10388, .T. ) ;
#8322 = CARTESIAN_POINT ( 'NONE',  ( 33.97500000054621694, 17.63344945572769973, 98.07665518445361386 ) ) ;
#8323 = LINE ( 'NONE', #6229, #272 ) ;
#8324 = CARTESIAN_POINT ( 'NONE',  ( 43.97500000054623115, 15.71886984736413417, 96.68563167572563088 ) ) ;
#8325 = CARTESIAN_POINT ( 'NONE',  ( 32.87500000054622262, 20.00000000000000355, 83.50966788445364841 ) ) ;
#8326 = CARTESIAN_POINT ( 'NONE',  ( 33.89999999999998437, 22.43689772174679575, 98.29316153445363113 ) ) ;
#8327 = VECTOR ( 'NONE', #8618, 1000.000000000000000 ) ;
#8328 = CARTESIAN_POINT ( 'NONE',  ( 10.00000000000000355, 20.00000000000000355, 22.91287847477919826 ) ) ;
#8329 = CARTESIAN_POINT ( 'NONE',  ( 40.27500000054623541, 12.34168156654572535, 90.79316153445363113 ) ) ;
#8330 = ORIENTED_EDGE ( 'NONE', *, *, #4417, .T. ) ;
#8331 = CARTESIAN_POINT ( 'NONE',  ( 45.87500000054622973, 17.63344945572769973, 98.07665518445361386 ) ) ;
#8332 = CARTESIAN_POINT ( 'NONE',  ( 28.45000000109246585, 15.59161060780646046, 84.72553407664153724 ) ) ;
#8333 = EDGE_LOOP ( 'NONE', ( #8070, #6318, #11392, #2233, #11138, #9588 ) ) ;
#8334 = CARTESIAN_POINT ( 'NONE',  ( -8.489225034269651360, 25.29515013360644460, 26.68274546775624145 ) ) ;
#8335 = VERTEX_POINT ( 'NONE', #3100 ) ;
#8336 = DIRECTION ( 'NONE',  ( -0.000000000000000000, -1.000000000000000000, -0.000000000000000000 ) ) ;
#8337 = CIRCLE ( 'NONE', #10348, 0.5999999999999998668 ) ;
#8338 = PLANE ( 'NONE',  #5667 ) ;
#8339 = CARTESIAN_POINT ( 'NONE',  ( 35.95000000109246940, 13.62011893735970958, 95.42841645007781892 ) ) ;
#8340 = CARTESIAN_POINT ( 'NONE',  ( 31.85000000109246443, 15.59161060780645691, 96.86078899226572503 ) ) ;
#8341 = CARTESIAN_POINT ( 'NONE',  ( 21.37500000054622618, 26.92701409722686634, 93.04388485072563242 ) ) ;
#8342 = CARTESIAN_POINT ( 'NONE',  ( 22.07500000054622191, 15.71886984736413417, 96.68563167572563088 ) ) ;
#8343 = CARTESIAN_POINT ( 'NONE',  ( 7.297108714790656592, 26.84519990999798367, 27.03346230006399509 ) ) ;
#8344 = DIRECTION ( 'NONE',  ( 0.000000000000000000, 0.000000000000000000, 1.000000000000000000 ) ) ;
#8345 = VERTEX_POINT ( 'NONE', #10840 ) ;
#8346 = CARTESIAN_POINT ( 'NONE',  ( 45.85000000109246798, 15.59161060780645691, 96.86078899226572503 ) ) ;
#8347 = CARTESIAN_POINT ( 'NONE',  ( -5.000000000000004441, 22.00000000000000000, 152.2284161474004520 ) ) ;
#8348 = ORIENTED_EDGE ( 'NONE', *, *, #5812, .F. ) ;
#8349 = CARTESIAN_POINT ( 'NONE',  ( 47.59999999999998721, 27.13292387221364876, 93.11078899226573924 ) ) ;
#8350 = ORIENTED_EDGE ( 'NONE', *, *, #7992, .T. ) ;
#8351 = DIRECTION ( 'NONE',  ( -0.000000000000000000, -0.000000000000000000, 1.000000000000000000 ) ) ;
#8352 = CARTESIAN_POINT ( 'NONE',  ( 6.000000000000000000, 0.000000000000000000, 0.000000000000000000 ) ) ;
#8353 = FACE_OUTER_BOUND ( 'NONE', #1491, .T. ) ;
#8354 = CARTESIAN_POINT ( 'NONE',  ( 5.000000000000000000, -4.685197434473812983, 6.938893903907228378E-15 ) ) ;
#8355 = CARTESIAN_POINT ( 'NONE',  ( 0.000000000000000000, 2.919948986426526005, -5.057500000000003659 ) ) ;
#8356 = LINE ( 'NONE', #3403, #4837 ) ;
#8357 = CARTESIAN_POINT ( 'NONE',  ( -0.3323029841801601880, 10.00000000000000711, 20.99999999999999645 ) ) ;
#8358 = CARTESIAN_POINT ( 'NONE',  ( 0.000000000000000000, 0.000000000000000000, 0.000000000000000000 ) ) ;
#8359 = EDGE_CURVE ( 'NONE', #6710, #5910, #7963, .T. ) ;
#8360 = CARTESIAN_POINT ( 'NONE',  ( 121.9999999999999858, 0.000000000000000000, 5.035999999999999588 ) ) ;
#8361 = CARTESIAN_POINT ( 'NONE',  ( -1.297965663867492347, 54.83959394270241461, 24.96833505342767978 ) ) ;
#8362 = ORIENTED_EDGE ( 'NONE', *, *, #8941, .F. ) ;
#8363 = CARTESIAN_POINT ( 'NONE',  ( 27.49999999999999645, 20.00000000000000355, 99.99999999999997158 ) ) ;
#8364 = CARTESIAN_POINT ( 'NONE',  ( 3.045782272221063902, 53.96862488584907425, 24.81409817615884705 ) ) ;
#8365 = CARTESIAN_POINT ( 'NONE',  ( 35.47500000054623115, 26.19570976099943493, 95.29460816699764791 ) ) ;
#8366 = CARTESIAN_POINT ( 'NONE',  ( 35.97500000054620983, 17.63344945572769973, 98.07665518445361386 ) ) ;
#8367 = CARTESIAN_POINT ( 'NONE',  ( 24.87500000054622618, 22.36655054427230382, 83.50966788445364841 ) ) ;
#8368 = CARTESIAN_POINT ( 'NONE',  ( 49.99999999999998579, 40.00000000000000000, 82.99999999999995737 ) ) ;
#8369 = DIRECTION ( 'NONE',  ( 0.000000000000000000, 0.4999999999999983902, -0.8660254037844395958 ) ) ;
#8370 = VECTOR ( 'NONE', #9077, 1000.000000000000000 ) ;
#8371 = LINE ( 'NONE', #1582, #9212 ) ;
#8372 = DIRECTION ( 'NONE',  ( 1.000000000000000000, -0.000000000000000000, -0.000000000000000000 ) ) ;
#8373 = ORIENTED_EDGE ( 'NONE', *, *, #2722, .T. ) ;
#8374 = DIRECTION ( 'NONE',  ( 1.000000000000000000, 0.000000000000000000, 0.000000000000000000 ) ) ;
#8375 = ORIENTED_EDGE ( 'NONE', *, *, #9707, .T. ) ;
#8376 = FACE_OUTER_BOUND ( 'NONE', #2962, .T. ) ;
#8377 = ADVANCED_FACE ( 'NONE', ( #9899 ), #11107, .F. ) ;
#8378 = VECTOR ( 'NONE', #10140, 1000.000000000000000 ) ;
#8379 = CARTESIAN_POINT ( 'NONE',  ( 33.57500000054622546, 26.19570976099943849, 95.29460816699764791 ) ) ;
#8380 = CARTESIAN_POINT ( 'NONE',  ( 27.15000000109246159, 27.88596668178699645, 90.79316153445363113 ) ) ;
#8381 = AXIS2_PLACEMENT_3D ( 'NONE', #10395, #10517, #10454 ) ;
#8382 = CARTESIAN_POINT ( 'NONE',  ( 46.67500000054623399, 17.63344945572770328, 83.50966788445364841 ) ) ;
#8383 = CARTESIAN_POINT ( 'NONE',  ( 33.47500000054622404, 26.92701409722686634, 93.04388485072563242 ) ) ;
#8384 = CARTESIAN_POINT ( 'NONE',  ( 30.69999999999998863, 13.62011893735971135, 86.15790661882942914 ) ) ;
#8385 = CARTESIAN_POINT ( 'NONE',  ( 0.6586899486374204749, 30.00000000000001421, 25.00000000000000000 ) ) ;
#8386 = CARTESIAN_POINT ( 'NONE',  ( 41.67500000054622689, 22.36655054427230027, 98.07665518445361386 ) ) ;
#8387 = ORIENTED_EDGE ( 'NONE', *, *, #4743, .T. ) ;
#8388 = CONICAL_SURFACE ( 'NONE', #9602, 5.035999999999999588, 0.7853981633974671528 ) ;
#8389 = CARTESIAN_POINT ( 'NONE',  ( 47.57500000054622546, 24.28113015263587116, 96.68563167572563088 ) ) ;
#8390 = DIRECTION ( 'NONE',  ( -1.000000000000000000, -0.000000000000000000, -0.000000000000000000 ) ) ;
#8391 = ORIENTED_EDGE ( 'NONE', *, *, #10849, .T. ) ;
#8392 = EDGE_CURVE ( 'NONE', #1420, #113, #6808, .T. ) ;
#8393 = CARTESIAN_POINT ( 'NONE',  ( 4.462820119357231441, 11.02737396841608586, 20.52942579431584846 ) ) ;
#8394 = ORIENTED_EDGE ( 'NONE', *, *, #11608, .F. ) ;
#8395 = CARTESIAN_POINT ( 'NONE',  ( 3.549343885166972523, 29.35473140773891032, -24.74867856782190856 ) ) ;
#8396 = DIRECTION ( 'NONE',  ( 1.000000000000000000, -0.000000000000000000, -0.000000000000000000 ) ) ;
#8397 = CARTESIAN_POINT ( 'NONE',  ( 49.99999999999998579, 20.00000000000000000, 145.0000000000000000 ) ) ;
#8398 = CYLINDRICAL_SURFACE ( 'NONE', #9211, 7.500000000000000000 ) ;
#8399 = EDGE_CURVE ( 'NONE', #6633, #10006, #3296, .T. ) ;
#8400 = CARTESIAN_POINT ( 'NONE',  ( 22.77500000054622831, 20.00000000000000355, 83.50966788445364841 ) ) ;
#8401 = CARTESIAN_POINT ( 'NONE',  ( 23.87500000054622262, 20.00000000000000355, 98.07665518445361386 ) ) ;
#8402 = AXIS2_PLACEMENT_3D ( 'NONE', #2703, #2892, #10498 ) ;
#8403 = CARTESIAN_POINT ( 'NONE',  ( 41.89999999999999147, 22.43689772174679575, 98.29316153445363113 ) ) ;
#8404 = CARTESIAN_POINT ( 'NONE',  ( -4.336726535208759614, 47.49029485220934532, 24.62166619875052831 ) ) ;
#8405 = ORIENTED_EDGE ( 'NONE', *, *, #10921, .T. ) ;
#8406 = CARTESIAN_POINT ( 'NONE',  ( 37.45000000109246230, 24.40838939219354842, 96.86078899226572503 ) ) ;
#8407 = CARTESIAN_POINT ( 'NONE',  ( 9.933637772289912959, 18.67556250305220189, 22.94215742280771408 ) ) ;
#8408 = EDGE_LOOP ( 'NONE', ( #5116, #9577, #4228, #7558 ) ) ;
#8409 = CARTESIAN_POINT ( 'NONE',  ( -2.000000000000015543, 20.00000000000000355, 98.29316153445363113 ) ) ;
#8410 = ORIENTED_EDGE ( 'NONE', *, *, #8511, .T. ) ;
#8411 = CARTESIAN_POINT ( 'NONE',  ( 44.65000000109246514, 20.00000000000000355, 83.29316153445364534 ) ) ;
#8412 = CARTESIAN_POINT ( 'NONE',  ( -5.000000000000000888, 18.00000000000000355, 169.9999999999999716 ) ) ;
#8413 = CARTESIAN_POINT ( 'NONE',  ( 0.000000000000000000, 0.000000000000000000, 8.400000000000000355 ) ) ;
#8414 = DIRECTION ( 'NONE',  ( 0.000000000000000000, 0.000000000000000000, -1.000000000000000000 ) ) ;
#8415 = ADVANCED_FACE ( 'NONE', ( #7160, #2404 ), #9202, .T. ) ;
#8416 = CARTESIAN_POINT ( 'NONE',  ( -34.72841614740048044, 18.00000000000000355, 169.9999999999999716 ) ) ;
#8417 = AXIS2_PLACEMENT_3D ( 'NONE', #9434, #10494, #6689 ) ;
#8418 = CARTESIAN_POINT ( 'NONE',  ( -6.124501814769208075, 12.06839632704649112, 20.09480714311373362 ) ) ;
#8419 = CARTESIAN_POINT ( 'NONE',  ( -5.837112373185870062, 11.87393669850012756, 27.38618981624034632 ) ) ;
#8420 = CARTESIAN_POINT ( 'NONE',  ( 22.67500000054622333, 17.63344945572770328, 83.50966788445364841 ) ) ;
#8421 = CARTESIAN_POINT ( 'NONE',  ( 7.298955741910466699, 26.84326632351102759, 23.91197098918000918 ) ) ;
#8422 = CARTESIAN_POINT ( 'NONE',  ( -6.999999999999964473, 20.00000000000000355, -70.00000000000000000 ) ) ;
#8423 = ORIENTED_EDGE ( 'NONE', *, *, #5440, .T. ) ;
#8424 = CARTESIAN_POINT ( 'NONE',  ( 3.061617023331388775E-15, 45.00000000000000711, 25.00000000000000000 ) ) ;
#8425 = EDGE_CURVE ( 'NONE', #9180, #1674, #12219, .T. ) ;
#8426 = DIRECTION ( 'NONE',  ( 0.000000000000000000, 0.000000000000000000, 1.000000000000000000 ) ) ;
#8427 = CARTESIAN_POINT ( 'NONE',  ( 35.77500000054622831, 20.00000000000000355, 98.07665518445361386 ) ) ;
#8428 = CARTESIAN_POINT ( 'NONE',  ( 35.87500000054622973, 20.00000000000000355, 98.07665518445361386 ) ) ;
#8429 = DIRECTION ( 'NONE',  ( 0.000000000000000000, -0.4999999999999983902, 0.8660254037844395958 ) ) ;
#8430 = CARTESIAN_POINT ( 'NONE',  ( 9.844533866065003025, 18.22526997752235189, 98.08466769849140121 ) ) ;
#8431 = FACE_OUTER_BOUND ( 'NONE', #6249, .T. ) ;
#8432 = CARTESIAN_POINT ( 'NONE',  ( 33.39999999999998437, 27.13292387221364876, 88.47553407664153724 ) ) ;
#8433 = CARTESIAN_POINT ( 'NONE',  ( 0.6000000000000033085, 1.028703311283776586E-15, -8.400000000000000355 ) ) ;
#8434 = CARTESIAN_POINT ( 'NONE',  ( -2.000000000000015543, 20.00000000000000355, 83.29316153445364534 ) ) ;
#8435 = ORIENTED_EDGE ( 'NONE', *, *, #10237, .T. ) ;
#8436 = CARTESIAN_POINT ( 'NONE',  ( 19.99999999999999645, 20.00000000000000355, 171.0000000000000000 ) ) ;
#8437 = DIRECTION ( 'NONE',  ( 0.000000000000000000, 0.000000000000000000, 1.000000000000000000 ) ) ;
#8438 = VECTOR ( 'NONE', #14, 1000.000000000000000 ) ;
#8439 =( BOUNDED_CURVE ( )  B_SPLINE_CURVE ( 3, ( #1906, #10412, #1783, #5789 ),
 .UNSPECIFIED., .F., .F. ) 
 B_SPLINE_CURVE_WITH_KNOTS ( ( 4, 4 ),
 ( 1.570796326794896558, 3.141592653589793560 ),
 .UNSPECIFIED. ) 
 CURVE ( )  GEOMETRIC_REPRESENTATION_ITEM ( )  RATIONAL_B_SPLINE_CURVE ( ( 1.000000000000000000, 0.8047378541243649375, 0.8047378541243649375, 1.000000000000000000 ) ) 
 REPRESENTATION_ITEM ( '' )  );
#8440 = CARTESIAN_POINT ( 'NONE',  ( 25.97500000054622049, 17.63344945572769973, 98.07665518445361386 ) ) ;
#8441 = LINE ( 'NONE', #2667, #8170 ) ;
#8442 = CARTESIAN_POINT ( 'NONE',  ( 48.27500000054622120, 12.34168156654572357, 90.79316153445363113 ) ) ;
#8443 = CARTESIAN_POINT ( 'NONE',  ( 31.37500000054622618, 27.65831843345427998, 90.79316153445363113 ) ) ;
#8444 = CARTESIAN_POINT ( 'NONE',  ( 27.69999999999998508, 26.37988106264029398, 95.42841645007781892 ) ) ;
#8445 = EDGE_CURVE ( 'NONE', #9490, #5989, #446, .T. ) ;
#8446 = CARTESIAN_POINT ( 'NONE',  ( 2.562745747226488176E-15, 30.00000000000001066, 21.00000000000000000 ) ) ;
#8447 = CARTESIAN_POINT ( 'NONE',  ( 36.57500000054622546, 15.71886984736413773, 84.90069139318163138 ) ) ;
#8448 = ORIENTED_EDGE ( 'NONE', *, *, #10768, .F. ) ;
#8449 = CARTESIAN_POINT ( 'NONE',  ( 49.37500000054622973, 26.92701409722686634, 93.04388485072563242 ) ) ;
#8450 = FACE_OUTER_BOUND ( 'NONE', #2505, .T. ) ;
#8451 = AXIS2_PLACEMENT_3D ( 'NONE', #872, #8611, #3660 ) ;
#8452 = ORIENTED_EDGE ( 'NONE', *, *, #8621, .F. ) ;
#8453 = APPLICATION_CONTEXT ( 'automotive_design' ) ;
#8454 = DIRECTION ( 'NONE',  ( 0.000000000000000000, 0.000000000000000000, 1.000000000000000000 ) ) ;
#8455 = EDGE_CURVE ( 'NONE', #11877, #9504, #1403, .T. ) ;
#8456 = ORIENTED_EDGE ( 'NONE', *, *, #4672, .T. ) ;
#8457 = LINE ( 'NONE', #4584, #11537 ) ;
#8458 = CARTESIAN_POINT ( 'NONE',  ( 1.612114502486744261, 45.25572168872454881, -27.95519462443614955 ) ) ;
#8459 = CARTESIAN_POINT ( 'NONE',  ( 49.82500000054622546, 20.00000000000000355, 98.29316153445363113 ) ) ;
#8460 = AXIS2_PLACEMENT_3D ( 'NONE', #9042, #4460, #4338 ) ;
#8461 = CARTESIAN_POINT ( 'NONE',  ( 25.27500000054622475, 27.65831843345427998, 90.79316153445363113 ) ) ;
#8462 = CARTESIAN_POINT ( 'NONE',  ( 20.87500000054622262, 20.00000000000000355, 83.50966788445364841 ) ) ;
#8463 = CARTESIAN_POINT ( 'NONE',  ( -5.033342733373901368, 28.66546597776486038, -24.49435860509168350 ) ) ;
#8464 = CARTESIAN_POINT ( 'NONE',  ( 5.000000000000000000, 2.342598717236912265, 4.057499999999998330 ) ) ;
#8465 = ORIENTED_EDGE ( 'NONE', *, *, #1424, .F. ) ;
#8466 = CARTESIAN_POINT ( 'NONE',  ( 37.85000000109246798, 15.59161060780645691, 96.86078899226572503 ) ) ;
#8467 = CARTESIAN_POINT ( 'NONE',  ( 2.221110608488543026, 54.49139573732541209, -24.90296241992962578 ) ) ;
#8468 = ORIENTED_EDGE ( 'NONE', *, *, #8321, .F. ) ;
#8469 = DIRECTION ( 'NONE',  ( 0.000000000000000000, 0.000000000000000000, -1.000000000000000000 ) ) ;
#8470 = EDGE_CURVE ( 'NONE', #5557, #9392, #10152, .T. ) ;
#8471 = EDGE_LOOP ( 'NONE', ( #10496, #11182, #10953 ) ) ;
#8472 = CARTESIAN_POINT ( 'NONE',  ( 3.050582886893512313, 53.97508389715062549, 20.77906331675102081 ) ) ;
#8473 = CARTESIAN_POINT ( 'NONE',  ( 5.318519735642854407, 11.52546059409457513, -20.31725095129150560 ) ) ;
#8474 = CARTESIAN_POINT ( 'NONE',  ( -10.00000000000000355, 20.00000000000000355, 22.91287847477919826 ) ) ;
#8475 = ADVANCED_FACE ( 'NONE', ( #3357 ), #7227, .T. ) ;
#8476 = VECTOR ( 'NONE', #9048, 1000.000000000000000 ) ;
#8477 = CARTESIAN_POINT ( 'NONE',  ( -31.74999999999995737, 0.000000000000000000, 5.000000000000000888 ) ) ;
#8478 = CARTESIAN_POINT ( 'NONE',  ( 41.99999999999998579, 20.00000000000000355, 98.29316153445363113 ) ) ;
#8479 = CARTESIAN_POINT ( 'NONE',  ( -50.00000000000001421, 20.00000000000000000, 145.0000000000000000 ) ) ;
#8480 = DIRECTION ( 'NONE',  ( 1.000000000000000000, 0.000000000000000000, 0.000000000000000000 ) ) ;
#8481 = CARTESIAN_POINT ( 'NONE',  ( 23.37500000054622973, 26.92701409722686634, 93.04388485072563242 ) ) ;
#8482 = CYLINDRICAL_SURFACE ( 'NONE', #725, 7.499999999999992895 ) ;
#8483 = CARTESIAN_POINT ( 'NONE',  ( -4.968274749745848595, 50.65218571871033504, 24.50144017370611493 ) ) ;
#8484 = VERTEX_POINT ( 'NONE', #8249 ) ;
#8485 = VECTOR ( 'NONE', #553, 1000.000000000000000 ) ;
#8486 = ORIENTED_EDGE ( 'NONE', *, *, #868, .T. ) ;
#8487 = CARTESIAN_POINT ( 'NONE',  ( 21.19999999999998508, 24.40838939219355197, 84.72553407664153724 ) ) ;
#8488 = DIRECTION ( 'NONE',  ( 0.000000000000000000, -0.000000000000000000, 1.000000000000000000 ) ) ;
#8489 = CARTESIAN_POINT ( 'NONE',  ( 40.87500000054622262, 20.00000000000000355, 83.50966788445364841 ) ) ;
#8490 = CARTESIAN_POINT ( 'NONE',  ( 21.87500000054622973, 17.63344945572769973, 98.07665518445361386 ) ) ;
#8491 = AXIS2_PLACEMENT_3D ( 'NONE', #2192, #4986, #2889 ) ;
#8492 = LINE ( 'NONE', #7605, #12335 ) ;
#8493 = CARTESIAN_POINT ( 'NONE',  ( 5.000000000000000000, 50.00000000000000000, -27.54995462791182703 ) ) ;
#8494 = DIRECTION ( 'NONE',  ( 0.000000000000000000, -0.7071067811865440200, 0.7071067811865511255 ) ) ;
#8495 = CARTESIAN_POINT ( 'NONE',  ( 1.615386348054266508, 45.25691898032514615, -20.93996090919613096 ) ) ;
#8496 = CLOSED_SHELL ( 'NONE', ( #8694, #10180, #8168, #1330, #2698, #3231, #4265, #8014, #679, #6983, #6577, #255, #9484, #1300, #12038, #11492, #3487, #3352, #9135, #1004, #4977, #9003, #10959, #8046, #2632, #5376, #4101 ) ) ;
#8497 = DIRECTION ( 'NONE',  ( -0.000000000000000000, 0.000000000000000000, 1.000000000000000000 ) ) ;
#8498 = ORIENTED_EDGE ( 'NONE', *, *, #10992, .T. ) ;
#8499 = DIRECTION ( 'NONE',  ( 1.000000000000000000, 0.000000000000000000, 0.000000000000000000 ) ) ;
#8500 = CARTESIAN_POINT ( 'NONE',  ( 25.07500000054622191, 24.28113015263587471, 84.90069139318163138 ) ) ;
#8501 = DIRECTION ( 'NONE',  ( 1.000000000000000000, 0.000000000000000000, 0.000000000000000000 ) ) ;
#8502 = CARTESIAN_POINT ( 'NONE',  ( 36.97500000054623115, 24.28113015263587471, 84.90069139318163138 ) ) ;
#8503 = CARTESIAN_POINT ( 'NONE',  ( 27.47500000054622404, 26.92701409722686634, 93.04388485072563242 ) ) ;
#8504 = CARTESIAN_POINT ( 'NONE',  ( 28.69999999999998863, 13.62011893735971135, 86.15790661882942914 ) ) ;
#8505 = DIRECTION ( 'NONE',  ( -0.4999999999999892308, -0.000000000000000000, -0.8660254037844448138 ) ) ;
#8506 = CARTESIAN_POINT ( 'NONE',  ( 39.07500000054621836, 26.19570976099943493, 86.29171490190961435 ) ) ;
#8507 = ORIENTED_EDGE ( 'NONE', *, *, #8455, .F. ) ;
#8508 = CARTESIAN_POINT ( 'NONE',  ( 49.07500000054622546, 26.19570976099943493, 86.29171490190961435 ) ) ;
#8509 = CARTESIAN_POINT ( 'NONE',  ( -4.335701919804127336, 47.48856945494961224, -20.54837457294841130 ) ) ;
#8510 = ORIENTED_EDGE ( 'NONE', *, *, #8941, .T. ) ;
#8511 = EDGE_CURVE ( 'NONE', #8002, #9150, #4187, .T. ) ;
#8512 = CARTESIAN_POINT ( 'NONE',  ( 1.321940027897182901, 10.06569995984262356, 20.96847759216316476 ) ) ;
#8513 = ORIENTED_EDGE ( 'NONE', *, *, #10927, .T. ) ;
#8514 =( BOUNDED_CURVE ( )  B_SPLINE_CURVE ( 2, ( #1771, #8123, #2089, #11932, #9841, #2025, #11870, #8881, #8951, #10845, #5908 ),
 .UNSPECIFIED., .F., .F. ) 
 B_SPLINE_CURVE_WITH_KNOTS ( ( 3, 2, 2, 2, 2, 3 ),
 ( 0.000000000000000000, 0.006666666666666673166, 0.01333333333333334633, 0.02000000000000001429, 0.02666666666666669266, 0.03333333333333336063 ),
 .UNSPECIFIED. ) 
 CURVE ( )  GEOMETRIC_REPRESENTATION_ITEM ( )  RATIONAL_B_SPLINE_CURVE ( ( 1.000000000000000000, 0.9510565162951535312, 1.000000000000000000, 0.9510565162951535312, 1.000000000000000000, 0.9510565162951535312, 1.000000000000000000, 0.9510565162951535312, 1.000000000000000000, 0.9510565162951533091, 1.000000000000000222 ) ) 
 REPRESENTATION_ITEM ( '' )  );
#8515 = CARTESIAN_POINT ( 'NONE',  ( -2.000000000000015543, 20.00000000000000355, 90.79316153445363113 ) ) ;
#8516 = DIRECTION ( 'NONE',  ( -1.000000000000000000, -0.000000000000000000, -0.000000000000000000 ) ) ;
#8517 = VECTOR ( 'NONE', #5073, 1000.000000000000000 ) ;
#8518 = CARTESIAN_POINT ( 'NONE',  ( 46.27500000054622831, 13.07298590277314254, 93.04388485072563242 ) ) ;
#8519 = LINE ( 'NONE', #8459, #2105 ) ;
#8520 = CARTESIAN_POINT ( 'NONE',  ( 43.47500000054622404, 26.92701409722686634, 93.04388485072563242 ) ) ;
#8521 = CARTESIAN_POINT ( 'NONE',  ( 45.89999999999999147, 22.43689772174679575, 98.29316153445363113 ) ) ;
#8522 = CARTESIAN_POINT ( 'NONE',  ( -3.709758735690515970E-18, 30.00000000000001066, -25.00000000000000000 ) ) ;
#8523 = CARTESIAN_POINT ( 'NONE',  ( 38.95000000109246230, 26.37988106264029398, 86.15790661882942914 ) ) ;
#8524 = ORIENTED_EDGE ( 'NONE', *, *, #6839, .F. ) ;
#8525 = CARTESIAN_POINT ( 'NONE',  ( 36.75000000109245946, 22.43689772174679575, 83.29316153445363113 ) ) ;
#8526 = CARTESIAN_POINT ( 'NONE',  ( 9.465993554759519313, 16.75899710733777326, 23.13883973029316010 ) ) ;
#8527 = ORIENTED_EDGE ( 'NONE', *, *, #12266, .T. ) ;
#8528 = CYLINDRICAL_SURFACE ( 'NONE', #390, 7.499999999999992895 ) ;
#8529 = VECTOR ( 'NONE', #6103, 1000.000000000000000 ) ;
#8530 = VERTEX_POINT ( 'NONE', #3481 ) ;
#8531 = DIRECTION ( 'NONE',  ( 0.000000000000000000, 0.000000000000000000, 1.000000000000000000 ) ) ;
#8532 = EDGE_CURVE ( 'NONE', #9642, #12368, #2529, .T. ) ;
#8533 = EDGE_CURVE ( 'NONE', #12151, #7564, #7288, .T. ) ;
#8534 = CYLINDRICAL_SURFACE ( 'NONE', #11909, 5.000000000000000000 ) ;
#8535 = CARTESIAN_POINT ( 'NONE',  ( -0.6600000499078774174, 29.98375368882421910, 24.99348755773349140 ) ) ;
#8536 = AXIS2_PLACEMENT_3D ( 'NONE', #696, #9458, #5712 ) ;
#8537 = ADVANCED_FACE ( 'NONE', ( #2463 ), #10207, .F. ) ;
#8538 = B_SPLINE_CURVE_WITH_KNOTS ( 'NONE', 3,
 ( #6518, #9571, #10896, #7917, #180, #9823, #4039, #3976, #11723, #8932, #2209, #11783, #10758, #10696, #307, #7854, #2069, #11663, #4102, #3088, #11849, #7980, #8045, #118, #3156, #8994, #51, #4171, #7022, #9760, #11914, #3221, #1069, #2969, #10964, #6955, #6081, #9951, #4932, #1257, #7791, #1200, #5067, #6835, #8800, #246, #5129, #7083, #2272, #2009, #6013, #6139, #10011, #4873 ),
 .UNSPECIFIED., .F., .F.,
 ( 4, 2, 2, 2, 2, 2, 2, 2, 2, 2, 2, 2, 2, 2, 2, 2, 2, 2, 2, 2, 2, 2, 2, 2, 2, 2, 4 ),
 ( 0.02456447672714493283, 0.02533051008357335709, 0.02609654344000177789, 0.02686257679643020216, 0.02762861015285862296, 0.02916067686571544720, 0.03069274357857226798, 0.03145877693500069572, 0.03222481029142912345, 0.03375687700428597893, 0.03452291036071443442, 0.03528894371714287603, 0.03605497707357133153, 0.03682101042999977314, 0.03758704378642822863, 0.03835307714285667025, 0.03988514385571360898, 0.04065117721214206448, 0.04141721056857051997, 0.04294927728142744483, 0.04371531063785590726, 0.04448134399428436969, 0.04601341070714128068, 0.04677944406356973617, 0.04754547741999817778, 0.04831151077642663327, 0.04907754413285508877 ),
 .UNSPECIFIED. ) ;
#8539 = DIRECTION ( 'NONE',  ( 0.000000000000000000, 0.000000000000000000, 1.000000000000000000 ) ) ;
#8540 = ADVANCED_BREP_SHAPE_REPRESENTATION ( '', ( #10384, #9021 ), #708 ) ;
#8541 = CARTESIAN_POINT ( 'NONE',  ( -50.00000000000001421, 20.00000000000000000, 137.5000000000000000 ) ) ;
#8542 = EDGE_LOOP ( 'NONE', ( #727, #10687, #8619, #11198 ) ) ;
#8543 = CARTESIAN_POINT ( 'NONE',  ( 6.000000000000000000, 2.919948986426540660, 5.057499999999996554 ) ) ;
#8544 = CARTESIAN_POINT ( 'NONE',  ( 3.429011039554510417E-15, 10.00000000000000000, 28.00000000000000355 ) ) ;
#8545 = CARTESIAN_POINT ( 'NONE',  ( 19.97500000054623115, 15.71886984736413417, 96.68563167572563088 ) ) ;
#8546 = CARTESIAN_POINT ( 'NONE',  ( 0.6000000000000033085, 0.000000000000000000, 0.000000000000000000 ) ) ;
#8547 = PLANE ( 'NONE',  #634 ) ;
#8548 = VERTEX_POINT ( 'NONE', #6400 ) ;
#8549 = EDGE_CURVE ( 'NONE', #801, #10915, #6156, .T. ) ;
#8550 = ORIENTED_EDGE ( 'NONE', *, *, #879, .T. ) ;
#8551 = CARTESIAN_POINT ( 'NONE',  ( 42.65000000109246514, 20.00000000000000355, 83.29316153445364534 ) ) ;
#8552 = CARTESIAN_POINT ( 'NONE',  ( 5.000000000000000000, 4.969004387540385421E-16, -4.057500000000000107 ) ) ;
#8553 = ADVANCED_FACE ( 'NONE', ( #10978 ), #10031, .F. ) ;
#8554 = CARTESIAN_POINT ( 'NONE',  ( 0.000000000000000000, -4.685197434473812983, 6.938893903907228378E-15 ) ) ;
#8555 = CARTESIAN_POINT ( 'NONE',  ( 49.82500000054622546, 20.00000000000000355, 98.07665518445361386 ) ) ;
#8556 = CARTESIAN_POINT ( 'NONE',  ( -3.973477254255321167, 53.05279027209265763, -20.62149924635092546 ) ) ;
#8557 = DIRECTION ( 'NONE',  ( 0.000000000000000000, 0.000000000000000000, -1.000000000000000000 ) ) ;
#8558 = CARTESIAN_POINT ( 'NONE',  ( -50.00000000000001421, 0.000000000000000000, 69.99999999999998579 ) ) ;
#8559 = LINE ( 'NONE', #8434, #6891 ) ;
#8560 = ORIENTED_EDGE ( 'NONE', *, *, #179, .F. ) ;
#8561 = SHAPE_REPRESENTATION ( 'socket head cap screw_iso_ISO 4762 M12 x 110 - 36N', ( #9021 ), #4332 ) ;
#8562 = CARTESIAN_POINT ( 'NONE',  ( -50.00000000000001421, 40.00000000000000000, 169.9999999999999716 ) ) ;
#8563 = APPLICATION_PROTOCOL_DEFINITION ( 'draft international standard', 'automotive_design', 1998, #4973 ) ;
#8564 = CARTESIAN_POINT ( 'NONE',  ( 29.25000000109246301, 27.13292387221364876, 93.11078899226573924 ) ) ;
#8565 = CIRCLE ( 'NONE', #1285, 6.000000000000000888 ) ;
#8566 = CARTESIAN_POINT ( 'NONE',  ( 36.57500000054622546, 15.71886984736413773, 84.90069139318163138 ) ) ;
#8567 = CARTESIAN_POINT ( 'NONE',  ( 29.17500000054622333, 26.19570976099943493, 86.29171490190961435 ) ) ;
#8568 = CARTESIAN_POINT ( 'NONE',  ( 26.99999999999998934, 20.00000000000000355, 83.29316153445364534 ) ) ;
#8569 = CARTESIAN_POINT ( 'NONE',  ( 30.19999999999998863, 15.59161060780645691, 96.86078899226572503 ) ) ;
#8570 = CARTESIAN_POINT ( 'NONE',  ( 40.77500000054622831, 20.00000000000000355, 83.50966788445364841 ) ) ;
#8571 = VERTEX_POINT ( 'NONE', #10265 ) ;
#8572 = CARTESIAN_POINT ( 'NONE',  ( 19.65000000109246514, 20.00000000000000355, 98.29316153445363113 ) ) ;
#8573 = CARTESIAN_POINT ( 'NONE',  ( -3.974164006894358003, 46.94850610908187605, -20.62134886892444641 ) ) ;
#8574 = EDGE_LOOP ( 'NONE', ( #8387, #6420, #9424, #6481, #8130 ) ) ;
#8575 = LINE ( 'NONE', #3745, #5092 ) ;
#8576 = EDGE_LOOP ( 'NONE', ( #2218, #3429, #10393, #1777 ) ) ;
#8577 = CARTESIAN_POINT ( 'NONE',  ( 10.00000000000000711, 20.65896320323604485, -22.91287847477919470 ) ) ;
#8578 = CARTESIAN_POINT ( 'NONE',  ( 5.340684424226280325E-17, 55.00000000000000000, -25.00000000000000000 ) ) ;
#8579 = CARTESIAN_POINT ( 'NONE',  ( 6.000000000000000000, 2.919948986426526005, -5.057500000000003659 ) ) ;
#8580 = CARTESIAN_POINT ( 'NONE',  ( 41.87500000054622262, 20.00000000000000355, 98.07665518445361386 ) ) ;
#8581 = LINE ( 'NONE', #9542, #4341 ) ;
#8582 = ADVANCED_FACE ( 'NONE', ( #8431 ), #11407, .F. ) ;
#8583 = CARTESIAN_POINT ( 'NONE',  ( 46.89999999999999147, 17.56310227825321135, 83.29316153445363113 ) ) ;
#8584 = PLANE ( 'NONE',  #9000 ) ;
#8585 = CARTESIAN_POINT ( 'NONE',  ( -4.967261190099589108, 49.34148114543111774, 24.50164489405593571 ) ) ;
#8586 = VERTEX_POINT ( 'NONE', #4618 ) ;
#8587 = AXIS2_PLACEMENT_3D ( 'NONE', #10272, #5469, #820 ) ;
#8588 = CARTESIAN_POINT ( 'NONE',  ( 39.35000000109246088, 26.37988106264029398, 95.42841645007781892 ) ) ;
#8589 = CARTESIAN_POINT ( 'NONE',  ( 0.000000000000000000, 8.878689293818310074E-16, -6.500000000000000888 ) ) ;
#8590 = ORIENTED_EDGE ( 'NONE', *, *, #5273, .T. ) ;
#8591 = DIRECTION ( 'NONE',  ( 1.000000000000000000, -0.000000000000000000, -0.000000000000000000 ) ) ;
#8592 = ORIENTED_EDGE ( 'NONE', *, *, #7609, .T. ) ;
#8593 = CARTESIAN_POINT ( 'NONE',  ( 11.99999999999999822, 0.000000000000000000, 0.000000000000000000 ) ) ;
#8594 = CARTESIAN_POINT ( 'NONE',  ( 7.945130733125017386, 13.89325898989267571, -19.44295271810430847 ) ) ;
#8595 = AXIS2_PLACEMENT_3D ( 'NONE', #4402, #5178, #2436 ) ;
#8596 = LINE ( 'NONE', #4603, #6359 ) ;
#8597 = CARTESIAN_POINT ( 'NONE',  ( -5.000000000000000000, 50.00000000000000000, 24.49489742783178414 ) ) ;
#8598 = DIRECTION ( 'NONE',  ( 0.000000000000000000, -1.000000000000000000, 0.000000000000000000 ) ) ;
#8599 = VERTEX_POINT ( 'NONE', #8493 ) ;
#8600 = EDGE_CURVE ( 'NONE', #10421, #6575, #36, .T. ) ;
#8601 = CARTESIAN_POINT ( 'NONE',  ( 27.65000000109246514, 20.00000000000000355, 98.29316153445363113 ) ) ;
#8602 = CARTESIAN_POINT ( 'NONE',  ( 6.000000000000000000, -5.258101095580059469E-15, -5.057500000000000995 ) ) ;
#8603 = CARTESIAN_POINT ( 'NONE',  ( 21.67500000054622689, 22.36655054427230027, 98.07665518445361386 ) ) ;
#8604 = ORIENTED_EDGE ( 'NONE', *, *, #5218, .T. ) ;
#8605 = CARTESIAN_POINT ( 'NONE',  ( 32.00000000000000000, 0.000000000000000000, 0.000000000000000000 ) ) ;
#8606 = VECTOR ( 'NONE', #5625, 1000.000000000000000 ) ;
#8607 = CARTESIAN_POINT ( 'NONE',  ( 23.29999999999998650, 26.37988106264029398, 86.15790661882942914 ) ) ;
#8608 = EDGE_LOOP ( 'NONE', ( #3271, #10623, #11670, #867, #9241, #8834 ) ) ;
#8609 = ORIENTED_EDGE ( 'NONE', *, *, #12193, .F. ) ;
#8610 = CARTESIAN_POINT ( 'NONE',  ( 0.6000000000000033085, 1.102182119232617714E-15, -9.000000000000000000 ) ) ;
#8611 = DIRECTION ( 'NONE',  ( 0.000000000000000000, 1.000000000000000000, 0.000000000000000000 ) ) ;
#8612 = AXIS2_PLACEMENT_3D ( 'NONE', #10369, #7648, #3646 ) ;
#8613 = CARTESIAN_POINT ( 'NONE',  ( 22.27500000054622475, 12.34168156654572357, 90.79316153445363113 ) ) ;
#8614 = FACE_OUTER_BOUND ( 'NONE', #3680, .T. ) ;
#8615 = CARTESIAN_POINT ( 'NONE',  ( -4.493388836263841668, 52.21708239239048055, -20.51403955935326096 ) ) ;
#8616 = LINE ( 'NONE', #3856, #10931 ) ;
#8617 = CARTESIAN_POINT ( 'NONE',  ( 3.764190923162284985, 46.69295727064967849, 27.74679428998945596 ) ) ;
#8618 = DIRECTION ( 'NONE',  ( -1.000000000000000000, -0.000000000000000000, -0.000000000000000000 ) ) ;
#8619 = ORIENTED_EDGE ( 'NONE', *, *, #5503, .T. ) ;
#8620 = LINE ( 'NONE', #8562, #439 ) ;
#8621 = EDGE_CURVE ( 'NONE', #2566, #9549, #2719, .T. ) ;
#8622 = ITEM_DEFINED_TRANSFORMATION ( 'NONE', 'NONE', #10806,  #9021 ) ;
#8623 = CARTESIAN_POINT ( 'NONE',  ( 26.47500000054622404, 13.07298590277314432, 88.54243821818161564 ) ) ;
#8624 = CARTESIAN_POINT ( 'NONE',  ( 36.49999999999998579, 12.11403331821300533, 90.79316153445363113 ) ) ;
#8625 = CARTESIAN_POINT ( 'NONE',  ( 41.17500000054623399, 26.92701409722686634, 88.54243821818162985 ) ) ;
#8626 = EDGE_CURVE ( 'NONE', #8287, #10068, #12240, .T. ) ;
#8627 = CARTESIAN_POINT ( 'NONE',  ( 26.67500000054622333, 15.71886984736413773, 84.90069139318163138 ) ) ;
#8628 = CARTESIAN_POINT ( 'NONE',  ( 28.39999999999998792, 12.86707612778636012, 93.11078899226572503 ) ) ;
#8629 = CYLINDRICAL_SURFACE ( 'NONE', #192, 5.000000000000000000 ) ;
#8630 = CARTESIAN_POINT ( 'NONE',  ( 35.77500000054622831, 20.00000000000000355, 98.07665518445361386 ) ) ;
#8631 = ORIENTED_EDGE ( 'NONE', *, *, #5505, .F. ) ;
#8632 = CARTESIAN_POINT ( 'NONE',  ( 45.27500000054622831, 27.65831843345427998, 90.79316153445363113 ) ) ;
#8633 = DIRECTION ( 'NONE',  ( 0.000000000000000000, 0.000000000000000000, 1.000000000000000000 ) ) ;
#8634 = ORIENTED_EDGE ( 'NONE', *, *, #2036, .T. ) ;
#8635 = DIRECTION ( 'NONE',  ( -0.5000000000000046629, 0.000000000000000000, 0.8660254037844359321 ) ) ;
#8636 = ORIENTED_EDGE ( 'NONE', *, *, #9724, .F. ) ;
#8637 = AXIS2_PLACEMENT_3D ( 'NONE', #9850, #3942, #8706 ) ;
#8638 = DIRECTION ( 'NONE',  ( 1.000000000000000000, -0.000000000000000000, -0.000000000000000000 ) ) ;
#8639 = CARTESIAN_POINT ( 'NONE',  ( 32.49999999999997868, 12.11403331821300533, 90.79316153445363113 ) ) ;
#8640 = CARTESIAN_POINT ( 'NONE',  ( 5.000000000000000000, 4.685197434473814759, -5.637851296924623057E-15 ) ) ;
#8641 = CARTESIAN_POINT ( 'NONE',  ( 45.07500000054622546, 24.28113015263587471, 84.90069139318163138 ) ) ;
#8642 = DIRECTION ( 'NONE',  ( 1.000000000000000000, 0.000000000000000000, 0.000000000000000000 ) ) ;
#8643 = DIRECTION ( 'NONE',  ( 1.000000000000000000, 0.000000000000000000, 0.000000000000000000 ) ) ;
#8644 = CARTESIAN_POINT ( 'NONE',  ( 46.67500000054622689, 15.71886984736413773, 84.90069139318163138 ) ) ;
#8645 = CARTESIAN_POINT ( 'NONE',  ( 47.89999999999999147, 22.43689772174679575, 98.29316153445363113 ) ) ;
#8646 = MECHANICAL_DESIGN_GEOMETRIC_PRESENTATION_REPRESENTATION (  '', ( #9065 ), #10466 ) ;
#8647 = CARTESIAN_POINT ( 'NONE',  ( 49.47500000054621694, 26.19570976099943493, 95.29460816699764791 ) ) ;
#8648 = ORIENTED_EDGE ( 'NONE', *, *, #5893, .F. ) ;
#8649 = CARTESIAN_POINT ( 'NONE',  ( 37.25000000109246656, 27.13292387221364876, 93.11078899226573924 ) ) ;
#8650 = CARTESIAN_POINT ( 'NONE',  ( 7.927224944456558120, 13.89552811154835510, 23.71088769051724654 ) ) ;
#8651 = EDGE_LOOP ( 'NONE', ( #2293, #6193, #767, #4642 ) ) ;
#8652 = SURFACE_STYLE_FILL_AREA ( #4659 ) ;
#8653 = ORIENTED_EDGE ( 'NONE', *, *, #4424, .F. ) ;
#8654 = EDGE_CURVE ( 'NONE', #11587, #8715, #11257, .T. ) ;
#8655 = DIRECTION ( 'NONE',  ( 0.000000000000000000, 0.000000000000000000, 1.000000000000000000 ) ) ;
#8656 = AXIS2_PLACEMENT_3D ( 'NONE', #8640, #5548, #718 ) ;
#8657 = CARTESIAN_POINT ( 'NONE',  ( 6.855064305785296241, 12.71219435950246712, -19.85111039280309342 ) ) ;
#8658 = CARTESIAN_POINT ( 'NONE',  ( -6.608338170980154302, 27.53359326989389189, 24.11557641055247458 ) ) ;
#8659 = CARTESIAN_POINT ( 'NONE',  ( 37.07500000054622546, 26.19570976099943493, 86.29171490190961435 ) ) ;
#8660 = PLANE ( 'NONE',  #6182 ) ;
#8661 = CARTESIAN_POINT ( 'NONE',  ( 27.29999999999998295, 26.37988106264029398, 86.15790661882942914 ) ) ;
#8662 = VERTEX_POINT ( 'NONE', #12098 ) ;
#8663 = DIRECTION ( 'NONE',  ( 1.000000000000000000, 0.000000000000000000, 0.000000000000000000 ) ) ;
#8664 = CARTESIAN_POINT ( 'NONE',  ( -31.74999999999995737, 7.347880794884123680E-16, -6.000000000000003553 ) ) ;
#8665 = CARTESIAN_POINT ( 'NONE',  ( 48.47500000054622404, 13.07298590277314432, 88.54243821818161564 ) ) ;
#8666 = CIRCLE ( 'NONE', #8637, 5.057500000000000107 ) ;
#8667 = ORIENTED_EDGE ( 'NONE', *, *, #1107, .F. ) ;
#8668 = DIRECTION ( 'NONE',  ( -0.000000000000000000, 0.000000000000000000, 1.000000000000000000 ) ) ;
#8669 = DIRECTION ( 'NONE',  ( 1.000000000000000000, -0.000000000000000000, -0.000000000000000000 ) ) ;
#8670 = ORIENTED_EDGE ( 'NONE', *, *, #3894, .F. ) ;
#8671 = ADVANCED_FACE ( 'NONE', ( #1445 ), #3191, .T. ) ;
#8672 = ORIENTED_EDGE ( 'NONE', *, *, #6220, .T. ) ;
#8673 = B_SPLINE_CURVE_WITH_KNOTS ( 'NONE', 3,
 ( #7342, #12232, #7220, #10316, #8180, #2458, #8305, #442, #4488, #5453, #4303, #3476, #11091, #6333, #4551, #11344, #2397, #8424 ),
 .UNSPECIFIED., .F., .F.,
 ( 4, 2, 2, 2, 2, 2, 2, 2, 4 ),
 ( 0.000000000000000000, 0.0009797303413002214287, 0.001959460682600442857, 0.002939191023900664286, 0.003918921365200885715, 0.004898651706501107143, 0.005878382047801328572, 0.006858112389101550001, 0.007837842730401771429 ),
 .UNSPECIFIED. ) ;
#8674 = CIRCLE ( 'NONE', #2593, 0.4000000000000001887 ) ;
#8675 = CARTESIAN_POINT ( 'NONE',  ( 43.65000000109246514, 20.00000000000000355, 98.29316153445363113 ) ) ;
#8676 = EDGE_CURVE ( 'NONE', #332, #12540, #6119, .T. ) ;
#8677 = DIRECTION ( 'NONE',  ( -1.000000000000000000, -0.000000000000000000, -0.000000000000000000 ) ) ;
#8678 = CARTESIAN_POINT ( 'NONE',  ( 19.97500000054623115, 15.71886984736413417, 96.68563167572563088 ) ) ;
#8679 = CARTESIAN_POINT ( 'NONE',  ( 27.49999999999999645, 20.00000000000000355, 189.9999999999999716 ) ) ;
#8680 = DIRECTION ( 'NONE',  ( 1.000000000000000000, 0.000000000000000000, 0.000000000000000000 ) ) ;
#8681 = DIRECTION ( 'NONE',  ( 1.000000000000000000, 0.000000000000000000, 0.000000000000000000 ) ) ;
#8682 = CARTESIAN_POINT ( 'NONE',  ( 9.099857169894804088, 24.15926487358204611, -18.92649755607681783 ) ) ;
#8683 = DIRECTION ( 'NONE',  ( -0.5000000000000034417, 0.000000000000000000, 0.8660254037844367092 ) ) ;
#8684 = EDGE_LOOP ( 'NONE', ( #7482, #7169, #8036, #1391 ) ) ;
#8685 = CARTESIAN_POINT ( 'NONE',  ( 0.3338900548043083893, 30.00000000000001066, -25.00000000000000355 ) ) ;
#8686 = UNCERTAINTY_MEASURE_WITH_UNIT (LENGTH_MEASURE( 1.000000000000000082E-05 ), #4130, 'distance_accuracy_value', 'NONE');
#8687 = SHAPE_DEFINITION_REPRESENTATION ( #1923, #8561 ) ;
#8688 = AXIS2_PLACEMENT_3D ( 'NONE', #1310, #5179, #524 ) ;
#8689 = CARTESIAN_POINT ( 'NONE',  ( 27.57500000054622191, 26.19570976099943849, 95.29460816699764791 ) ) ;
#8690 = CARTESIAN_POINT ( 'NONE',  ( 24.05000000109246372, 12.86707612778636012, 93.11078899226572503 ) ) ;
#8691 = CARTESIAN_POINT ( 'NONE',  ( 39.77500000054622831, 20.00000000000000355, 98.07665518445361386 ) ) ;
#8692 = CARTESIAN_POINT ( 'NONE',  ( 27.67500000054622333, 24.28113015263587116, 96.68563167572563088 ) ) ;
#8693 = CARTESIAN_POINT ( 'NONE',  ( 24.79999999999999005, 15.59161060780646046, 84.72553407664153724 ) ) ;
#8694 = ADVANCED_FACE ( 'NONE', ( #2446 ), #161, .F. ) ;
#8695 = LINE ( 'NONE', #7619, #5662 ) ;
#8696 = CARTESIAN_POINT ( 'NONE',  ( 34.77500000054622831, 20.00000000000000355, 83.50966788445364841 ) ) ;
#8697 = ORIENTED_EDGE ( 'NONE', *, *, #7111, .F. ) ;
#8698 = PLANE ( 'NONE',  #1022 ) ;
#8699 = VERTEX_POINT ( 'NONE', #11200 ) ;
#8700 = CARTESIAN_POINT ( 'NONE',  ( 49.65000000109246514, 20.00000000000000355, 98.29316153445363113 ) ) ;
#8701 = EDGE_CURVE ( 'NONE', #4128, #4353, #1381, .T. ) ;
#8702 = ORIENTED_EDGE ( 'NONE', *, *, #5303, .T. ) ;
#8703 = EDGE_CURVE ( 'NONE', #1560, #10888, #7392, .T. ) ;
#8704 = VECTOR ( 'NONE', #8022, 1000.000000000000000 ) ;
#8705 = CARTESIAN_POINT ( 'NONE',  ( 43.39999999999998437, 27.13292387221364876, 88.47553407664153724 ) ) ;
#8706 = DIRECTION ( 'NONE',  ( 0.000000000000000000, 0.000000000000000000, 1.000000000000000000 ) ) ;
#8707 = DIRECTION ( 'NONE',  ( 0.000000000000000000, 0.000000000000000000, -1.000000000000000000 ) ) ;
#8708 =( NAMED_UNIT ( * ) SI_UNIT ( $, .STERADIAN. ) SOLID_ANGLE_UNIT ( ) );
#8709 = CARTESIAN_POINT ( 'NONE',  ( 49.69999999999998863, 26.37988106264029398, 95.42841645007781892 ) ) ;
#8710 = CARTESIAN_POINT ( 'NONE',  ( -9.355575343945487177, 23.54668771876638189, -23.18385937405269459 ) ) ;
#8711 = CARTESIAN_POINT ( 'NONE',  ( 44.69999999999998153, 13.62011893735970958, 86.15790661882942914 ) ) ;
#8712 = EDGE_LOOP ( 'NONE', ( #4094, #10451, #6984, #5288, #10655, #2957, #4678, #592, #11995, #5291, #4926, #4864, #983, #4535, #8667, #3193 ) ) ;
#8713 = CARTESIAN_POINT ( 'NONE',  ( 31.55000000109246727, 22.43689772174679575, 98.29316153445363113 ) ) ;
#8714 = CARTESIAN_POINT ( 'NONE',  ( 1.314997555680467389, 10.06486170053814533, 24.97384176433527969 ) ) ;
#8715 = VERTEX_POINT ( 'NONE', #1864 ) ;
#8716 = VERTEX_POINT ( 'NONE', #4724 ) ;
#8717 = CONICAL_SURFACE ( 'NONE', #11968, 4.057500000000000107, 1.047197551196593857 ) ;
#8718 = DIRECTION ( 'NONE',  ( 0.000000000000000000, 1.000000000000000000, -1.039664082171044875E-15 ) ) ;
#8719 = CARTESIAN_POINT ( 'NONE',  ( 89.17200000000001125, 0.000000000000000000, 0.000000000000000000 ) ) ;
#8720 = LINE ( 'NONE', #33, #10204 ) ;
#8721 = CARTESIAN_POINT ( 'NONE',  ( 35.17500000054622689, 26.92701409722686634, 88.54243821818162985 ) ) ;
#8722 = CARTESIAN_POINT ( 'NONE',  ( 34.97500000054622404, 22.36655054427230382, 83.50966788445364841 ) ) ;
#8723 = CARTESIAN_POINT ( 'NONE',  ( 8.675702521724353744, 25.01627270855146534, -26.62476894046449161 ) ) ;
#8724 = DIRECTION ( 'NONE',  ( -1.000000000000000000, -0.000000000000000000, -0.000000000000000000 ) ) ;
#8725 = EDGE_LOOP ( 'NONE', ( #10568, #10037, #7621, #8631, #664, #1617, #9906, #10515, #7830 ) ) ;
#8726 = AXIS2_PLACEMENT_3D ( 'NONE', #9271, #6524, #10328 ) ;
#8727 = CARTESIAN_POINT ( 'NONE',  ( 0.6566478411514924396, 54.96742651404818503, -27.99413128707798037 ) ) ;
#8728 = FACE_OUTER_BOUND ( 'NONE', #2339, .T. ) ;
#8729 = ORIENTED_EDGE ( 'NONE', *, *, #2062, .F. ) ;
#8730 = DIRECTION ( 'NONE',  ( -1.000000000000000000, -0.000000000000000000, -0.000000000000000000 ) ) ;
#8731 = CARTESIAN_POINT ( 'NONE',  ( 10.40000000000000036, 0.000000000000000000, 0.000000000000000000 ) ) ;
#8732 = ORIENTED_EDGE ( 'NONE', *, *, #1344, .F. ) ;
#8733 = ORIENTED_EDGE ( 'NONE', *, *, #3417, .T. ) ;
#8734 = AXIS2_PLACEMENT_3D ( 'NONE', #7876, #5787, #1036 ) ;
#8735 = CARTESIAN_POINT ( 'NONE',  ( 43.35000000109246088, 26.37988106264029398, 95.42841645007781892 ) ) ;
#8736 = LINE ( 'NONE', #4872, #10877 ) ;
#8737 = CARTESIAN_POINT ( 'NONE',  ( -50.00000000000001421, 40.00000000000000000, 169.9999999999999716 ) ) ;
#8738 = EDGE_CURVE ( 'NONE', #3840, #5684, #562, .T. ) ;
#8739 = CARTESIAN_POINT ( 'NONE',  ( 37.89999999999999147, 22.43689772174674246, 98.29316153445367377 ) ) ;
#8740 = FACE_BOUND ( 'NONE', #7561, .T. ) ;
#8741 = CARTESIAN_POINT ( 'NONE',  ( 0.3269974554053095006, 45.00000000000000711, -20.99999999999999289 ) ) ;
#8742 = CARTESIAN_POINT ( 'NONE',  ( 7.929954359405766873, 26.10079283832167008, -19.44644565266314373 ) ) ;
#8743 = CARTESIAN_POINT ( 'NONE',  ( 2.610381677634093123, 10.34108370468245219, 24.86537221636008965 ) ) ;
#8744 = EDGE_LOOP ( 'NONE', ( #6008, #11842, #10376, #5272 ) ) ;
#8745 = CARTESIAN_POINT ( 'NONE',  ( 6.601689117734505174, 27.51820487403981375, -24.11400268645312650 ) ) ;
#8746 = CARTESIAN_POINT ( 'NONE',  ( 46.49999999999998579, 12.11403331821300533, 90.79316153445363113 ) ) ;
#8747 = CARTESIAN_POINT ( 'NONE',  ( 48.97500000054622404, 22.36655054427230382, 83.50966788445364841 ) ) ;
#8748 = CARTESIAN_POINT ( 'NONE',  ( 37.27500000054622831, 27.65831843345427998, 90.79316153445363113 ) ) ;
#8749 = CARTESIAN_POINT ( 'NONE',  ( 22.87500000054622618, 20.00000000000000355, 83.50966788445364841 ) ) ;
#8750 = CARTESIAN_POINT ( 'NONE',  ( 21.99999999999998934, 20.00000000000000355, 98.29316153445363113 ) ) ;
#8751 = CARTESIAN_POINT ( 'NONE',  ( 34.29999999999996874, 13.62011893735970958, 95.42841645007781892 ) ) ;
#8752 = CARTESIAN_POINT ( 'NONE',  ( 31.57500000054622902, 24.28113015263587116, 96.68563167572563088 ) ) ;
#8753 = ORIENTED_EDGE ( 'NONE', *, *, #10775, .F. ) ;
#8754 = EDGE_CURVE ( 'NONE', #5847, #58, #9413, .T. ) ;
#8755 = DIRECTION ( 'NONE',  ( -1.000000000000000000, 0.000000000000000000, 0.000000000000000000 ) ) ;
#8756 = VERTEX_POINT ( 'NONE', #8412 ) ;
#8757 = CARTESIAN_POINT ( 'NONE',  ( 49.05000000109246372, 27.13292387221364876, 88.47553407664153724 ) ) ;
#8758 = EDGE_LOOP ( 'NONE', ( #6824, #9983, #937, #5896, #3972, #11743 ) ) ;
#8759 =( NAMED_UNIT ( * ) PLANE_ANGLE_UNIT ( ) SI_UNIT ( $, .RADIAN. ) );
#8760 = LINE ( 'NONE', #1039, #940 ) ;
#8761 = CARTESIAN_POINT ( 'NONE',  ( 4.437260769980855279, 11.03236584733799930, -27.64772768517902790 ) ) ;
#8762 = CARTESIAN_POINT ( 'NONE',  ( 45.67500000054621978, 24.28113015263587116, 96.68563167572563088 ) ) ;
#8763 = CARTESIAN_POINT ( 'NONE',  ( -111.8465843842649292, 69.50000000000000000, 146.8533255156881978 ) ) ;
#8764 = LINE ( 'NONE', #3819, #8256 ) ;
#8765 = CARTESIAN_POINT ( 'NONE',  ( 44.97500000054621694, 22.36655054427230382, 83.50966788445364841 ) ) ;
#8766 = CARTESIAN_POINT ( 'NONE',  ( 41.89999999999999858, 22.43689772174679575, 98.29316153445363113 ) ) ;
#8767 = CARTESIAN_POINT ( 'NONE',  ( 39.49999999999997868, 27.88596668178699645, 90.79316153445363113 ) ) ;
#8768 = LINE ( 'NONE', #2176, #11319 ) ;
#8769 = ORIENTED_EDGE ( 'NONE', *, *, #12103, .T. ) ;
#8770 = ADVANCED_FACE ( 'NONE', ( #6563 ), #10491, .F. ) ;
#8771 = VECTOR ( 'NONE', #6472, 1000.000000000000000 ) ;
#8772 = CARTESIAN_POINT ( 'NONE',  ( 33.55000000109246372, 22.43689772174679575, 98.29316153445363113 ) ) ;
#8773 = CARTESIAN_POINT ( 'NONE',  ( 0.000000000000000000, 0.000000000000000000, 0.000000000000000000 ) ) ;
#8774 = ORIENTED_EDGE ( 'NONE', *, *, #8202, .F. ) ;
#8775 = ORIENTED_EDGE ( 'NONE', *, *, #7153, .F. ) ;
#8776 = CARTESIAN_POINT ( 'NONE',  ( -10.00000000000000355, 20.00000000000000355, -22.91287847477919826 ) ) ;
#8777 = EDGE_CURVE ( 'NONE', #6575, #12211, #10555, .T. ) ;
#8778 = CARTESIAN_POINT ( 'NONE',  ( -4.339203347172030156, 52.50587310092982563, -24.62124401584528499 ) ) ;
#8779 = CARTESIAN_POINT ( 'NONE',  ( 27.49999999999999645, 20.00000000000000355, 162.0000000000000000 ) ) ;
#8780 = AXIS2_PLACEMENT_3D ( 'NONE', #170, #2060, #9687 ) ;
#8781 = CARTESIAN_POINT ( 'NONE',  ( 39.17500000054623399, 26.92701409722686634, 88.54243821818162985 ) ) ;
#8782 = CARTESIAN_POINT ( 'NONE',  ( 32.27500000054622831, 13.07298590277314254, 93.04388485072563242 ) ) ;
#8783 = DIRECTION ( 'NONE',  ( 0.000000000000000000, 0.000000000000000000, 1.000000000000000000 ) ) ;
#8784 = CARTESIAN_POINT ( 'NONE',  ( 35.65000000109246514, 20.00000000000000355, 98.29316153445363113 ) ) ;
#8785 = ADVANCED_FACE ( 'NONE', ( #5687 ), #8534, .F. ) ;
#8786 = LINE ( 'NONE', #11769, #9706 ) ;
#8787 = CARTESIAN_POINT ( 'NONE',  ( 53.00000000000000711, 20.00000000000000711, 189.9999999999999716 ) ) ;
#8788 = EDGE_LOOP ( 'NONE', ( #11491, #4689, #6132, #5782 ) ) ;
#8789 = CARTESIAN_POINT ( 'NONE',  ( 4.339699721346885752, 52.50479725378321660, -24.62114839412567235 ) ) ;
#8790 = LINE ( 'NONE', #6005, #12261 ) ;
#8791 = ORIENTED_EDGE ( 'NONE', *, *, #7111, .T. ) ;
#8792 = LINE ( 'NONE', #9815, #339 ) ;
#8793 = CIRCLE ( 'NONE', #3323, 5.057500000000000107 ) ;
#8794 = EDGE_LOOP ( 'NONE', ( #8955, #6393 ) ) ;
#8795 = AXIS2_PLACEMENT_3D ( 'NONE', #3511, #2686, #7382 ) ;
#8796 = EDGE_LOOP ( 'NONE', ( #9927, #5352, #3020, #4125 ) ) ;
#8797 = CARTESIAN_POINT ( 'NONE',  ( 6.000000000000000000, -2.919948986426525117, 5.057500000000004547 ) ) ;
#8798 = EDGE_CURVE ( 'NONE', #7546, #8162, #4741, .T. ) ;
#8799 = CARTESIAN_POINT ( 'NONE',  ( 5.000000000000000000, -2.342598717236902051, 4.057500000000004547 ) ) ;
#8800 = CARTESIAN_POINT ( 'NONE',  ( 9.405136654060040513, 23.43083853196268507, 84.10547354511845697 ) ) ;
#8801 = CARTESIAN_POINT ( 'NONE',  ( 37.49999999999999289, 27.88596668178699645, 90.79316153445363113 ) ) ;
#8802 = CIRCLE ( 'NONE', #9615, 7.499999999999978684 ) ;
#8803 = CARTESIAN_POINT ( 'NONE',  ( -4.744081181139592651, 48.38712208294071360, -24.54608042500704457 ) ) ;
#8804 = DIRECTION ( 'NONE',  ( 0.000000000000000000, 0.000000000000000000, 1.000000000000000000 ) ) ;
#8805 = LINE ( 'NONE', #9576, #11356 ) ;
#8806 = ORIENTED_EDGE ( 'NONE', *, *, #1174, .F. ) ;
#8807 = CARTESIAN_POINT ( 'NONE',  ( 4.462630933173456604, 28.97330998342967234, -24.60619142875309251 ) ) ;
#8808 = EDGE_CURVE ( 'NONE', #4258, #8883, #12161, .T. ) ;
#8809 = AXIS2_PLACEMENT_3D ( 'NONE', #1355, #2241, #5221 ) ;
#8810 = CARTESIAN_POINT ( 'NONE',  ( 46.29999999999999005, 13.62011893735970958, 95.42841645007781892 ) ) ;
#8811 = CARTESIAN_POINT ( 'NONE',  ( 23.75000000109246301, 17.56310227825320425, 98.29316153445363113 ) ) ;
#8812 = CARTESIAN_POINT ( 'NONE',  ( 30.57500000054622902, 15.71886984736413773, 84.90069139318163138 ) ) ;
#8813 = CARTESIAN_POINT ( 'NONE',  ( 3.246557057937244029, 10.51899376542992925, -24.79585947768713439 ) ) ;
#8814 = CARTESIAN_POINT ( 'NONE',  ( 22.09999999999998010, 17.56310227825320425, 98.29316153445363113 ) ) ;
#8815 = CARTESIAN_POINT ( 'NONE',  ( 5.000000000000000000, -4.506943796211478080E-15, -4.057500000000000107 ) ) ;
#8816 = CARTESIAN_POINT ( 'NONE',  ( 34.27500000054623541, 12.34168156654572535, 90.79316153445363113 ) ) ;
#8817 = EDGE_LOOP ( 'NONE', ( #11288, #6209, #5309, #5039 ) ) ;
#8818 = PRODUCT_DEFINITION_SHAPE ( 'NONE', 'NONE',  #12556 ) ;
#8819 = DIRECTION ( 'NONE',  ( 0.000000000000000000, 0.000000000000000000, -1.000000000000000000 ) ) ;
#8820 = ORIENTED_EDGE ( 'NONE', *, *, #10306, .F. ) ;
#8821 = CARTESIAN_POINT ( 'NONE',  ( 19.82500000054622546, 20.00000000000000355, 98.29316153445363113 ) ) ;
#8822 = VERTEX_POINT ( 'NONE', #10677 ) ;
#8823 = CARTESIAN_POINT ( 'NONE',  ( -4.339203347172030156, 52.50587310092982563, -24.62124401584528499 ) ) ;
#8824 = CARTESIAN_POINT ( 'NONE',  ( 6.607022230516116146, 12.46548842210657426, -27.21346531667574098 ) ) ;
#8825 = B_SPLINE_CURVE_WITH_KNOTS ( 'NONE', 3,
 ( #375, #435, #3527, #8174, #1387, #10197, #2391, #11146, #2453, #9127, #4298, #12043, #6327, #11205, #4419, #1872, #8419, #5753, #6694, #10372, #1810, #4673, #10434, #1685, #9562, #11395, #9624, #8544 ),
 .UNSPECIFIED., .F., .F.,
 ( 4, 2, 2, 2, 2, 2, 2, 2, 2, 2, 2, 2, 2, 4 ),
 ( 0.03152606207563762863, 0.03251081260015469682, 0.03349556312467176500, 0.03546506417370590136, 0.03644981469822297648, 0.03743456522274005160, 0.03940406627177420185, 0.04038881679629127003, 0.04137356732080833821, 0.04235831784532541333, 0.04334306836984248845, 0.04531256941887662482, 0.04629731994339369994, 0.04728207046791076812 ),
 .UNSPECIFIED. ) ;
#8826 = CARTESIAN_POINT ( 'NONE',  ( 35.97500000054620983, 17.63344945572769973, 98.07665518445361386 ) ) ;
#8827 = PLANE ( 'NONE',  #11401 ) ;
#8828 = EDGE_CURVE ( 'NONE', #10247, #1426, #11703, .T. ) ;
#8829 = CARTESIAN_POINT ( 'NONE',  ( 10.00000000000000355, 20.00000000000000355, 98.29316153445363113 ) ) ;
#8830 = CARTESIAN_POINT ( 'NONE',  ( 37.07500000054622546, 24.28113015263587471, 84.90069139318163138 ) ) ;
#8831 = CARTESIAN_POINT ( 'NONE',  ( 42.19999999999998863, 15.59161060780645691, 96.86078899226572503 ) ) ;
#8832 = CARTESIAN_POINT ( 'NONE',  ( 45.79999999999999005, 24.40838939219354842, 96.86078899226572503 ) ) ;
#8833 = CARTESIAN_POINT ( 'NONE',  ( 44.49999999999999289, 12.11403331821300533, 90.79316153445363113 ) ) ;
#8834 = ORIENTED_EDGE ( 'NONE', *, *, #764, .T. ) ;
#8835 = ADVANCED_FACE ( 'NONE', ( #8908 ), #4980, .F. ) ;
#8836 = CARTESIAN_POINT ( 'NONE',  ( 29.65000000109246514, 20.00000000000000355, 98.29316153445363113 ) ) ;
#8837 = CARTESIAN_POINT ( 'NONE',  ( 6.000000000000000000, -5.839897972853060892, 7.806255641895631925E-15 ) ) ;
#8838 = ORIENTED_EDGE ( 'NONE', *, *, #8738, .F. ) ;
#8839 = EDGE_LOOP ( 'NONE', ( #1019, #7765, #3561, #6101 ) ) ;
#8840 = CYLINDRICAL_SURFACE ( 'NONE', #6834, 7.499999999999978684 ) ;
#8841 = LINE ( 'NONE', #99, #10014 ) ;
#8842 = CIRCLE ( 'NONE', #8040, 8.400000000000000355 ) ;
#8843 =( BOUNDED_CURVE ( )  B_SPLINE_CURVE ( 2, ( #9018, #12122, #7292, #11935, #1220, #3180, #3300, #5151, #10035, #10916, #6100 ),
 .UNSPECIFIED., .F., .F. ) 
 B_SPLINE_CURVE_WITH_KNOTS ( ( 3, 2, 2, 2, 2, 3 ),
 ( 0.8666666666666666963, 0.8733333333333332948, 0.8800000000000000044, 0.8866666666666667140, 0.8933333333333333126, 0.9000000000000000222 ),
 .UNSPECIFIED. ) 
 CURVE ( )  GEOMETRIC_REPRESENTATION_ITEM ( )  RATIONAL_B_SPLINE_CURVE ( ( 1.000000000000000000, 0.9510565162951535312, 1.000000000000000000, 0.9510565162951535312, 1.000000000000000000, 0.9510565162951535312, 1.000000000000000000, 0.9510565162951535312, 1.000000000000000000, 0.9510565162951535312, 1.000000000000000000 ) ) 
 REPRESENTATION_ITEM ( '' )  );
#8844 = CARTESIAN_POINT ( 'NONE',  ( 33.77500000054622831, 20.00000000000000355, 98.07665518445361386 ) ) ;
#8845 = CARTESIAN_POINT ( 'NONE',  ( 31.47500000054622404, 26.92701409722686634, 93.04388485072563242 ) ) ;
#8846 = CARTESIAN_POINT ( 'NONE',  ( 5.840594436583858240, 28.12365591114656738, -27.38546733845194936 ) ) ;
#8847 = LINE ( 'NONE', #5427, #2394 ) ;
#8848 = ORIENTED_EDGE ( 'NONE', *, *, #11416, .T. ) ;
#8849 = CARTESIAN_POINT ( 'NONE',  ( 48.47500000054622404, 13.07298590277314432, 88.54243821818161564 ) ) ;
#8850 = EDGE_CURVE ( 'NONE', #730, #9626, #7769, .T. ) ;
#8851 = CARTESIAN_POINT ( 'NONE',  ( 47.75000000109245946, 17.56310227825320425, 98.29316153445363113 ) ) ;
#8852 = DIRECTION ( 'NONE',  ( -1.000000000000000000, -0.000000000000000000, -0.000000000000000000 ) ) ;
#8853 = ORIENTED_EDGE ( 'NONE', *, *, #8445, .F. ) ;
#8854 = DIRECTION ( 'NONE',  ( 1.000000000000000000, 0.000000000000000000, 0.000000000000000000 ) ) ;
#8855 = ORIENTED_EDGE ( 'NONE', *, *, #4672, .F. ) ;
#8856 = AXIS2_PLACEMENT_3D ( 'NONE', #9186, #11912, #8107 ) ;
#8857 = APPLICATION_CONTEXT ( 'automotive_design' ) ;
#8858 = CARTESIAN_POINT ( 'NONE',  ( -5.000000000000000888, 0.000000000000000000, 121.2488769092545198 ) ) ;
#8859 = VERTEX_POINT ( 'NONE', #3007 ) ;
#8860 = ADVANCED_FACE ( 'NONE', ( #10802 ), #11896, .T. ) ;
#8861 = ADVANCED_FACE ( 'NONE', ( #987 ), #3959, .F. ) ;
#8862 = CARTESIAN_POINT ( 'NONE',  ( 34.99999999999999289, 20.00000000000000355, 83.29316153445364534 ) ) ;
#8863 = CARTESIAN_POINT ( 'NONE',  ( 0.6550203249928933102, 54.96765362015771927, 24.99347278016167095 ) ) ;
#8864 = VECTOR ( 'NONE', #1549, 1000.000000000000000 ) ;
#8865 = CARTESIAN_POINT ( 'NONE',  ( 21.20617189303578698, 25.37779564132840804, 151.2938281069642130 ) ) ;
#8866 = CARTESIAN_POINT ( 'NONE',  ( 37.09999999999998010, 22.43689772174681707, 83.29316153445364534 ) ) ;
#8867 = CARTESIAN_POINT ( 'NONE',  ( -1.301064515050044168, 45.16113941612564275, -24.96819193944210724 ) ) ;
#8868 = CYLINDRICAL_SURFACE ( 'NONE', #6952, 7.499999999999992895 ) ;
#8869 = CARTESIAN_POINT ( 'NONE',  ( 6.000000000000000000, 5.839897972853065333, -6.938893903907228378E-15 ) ) ;
#8870 = CARTESIAN_POINT ( 'NONE',  ( 40.87500000054623683, 22.36655054427230382, 83.50966788445364841 ) ) ;
#8871 = DIRECTION ( 'NONE',  ( 0.000000000000000000, 0.000000000000000000, 1.000000000000000000 ) ) ;
#8872 = ORIENTED_EDGE ( 'NONE', *, *, #6277, .F. ) ;
#8873 = DIRECTION ( 'NONE',  ( 1.000000000000000000, 0.000000000000000000, 0.000000000000000000 ) ) ;
#8874 = APPLICATION_PROTOCOL_DEFINITION ( 'draft international standard', 'automotive_design', 1998, #1721 ) ;
#8875 = CARTESIAN_POINT ( 'NONE',  ( 21.67500000054622333, 24.28113015263587116, 96.68563167572563088 ) ) ;
#8876 = CARTESIAN_POINT ( 'NONE',  ( 24.55000000109246017, 17.56310227825320425, 83.29316153445363113 ) ) ;
#8877 = CARTESIAN_POINT ( 'NONE',  ( 30.07500000054622546, 13.80429023900056507, 95.29460816699764791 ) ) ;
#8878 = AXIS2_PLACEMENT_3D ( 'NONE', #11648, #2193, #3014 ) ;
#8879 = CARTESIAN_POINT ( 'NONE',  ( 22.07500000054622191, 15.71886984736413417, 96.68563167572563088 ) ) ;
#8880 = CARTESIAN_POINT ( 'NONE',  ( 26.19999999999998863, 15.59161060780645691, 96.86078899226572503 ) ) ;
#8881 = CARTESIAN_POINT ( 'NONE',  ( 49.29999999999998295, 26.37988106264029398, 86.15790661882942914 ) ) ;
#8882 = CARTESIAN_POINT ( 'NONE',  ( 35.97500000054623115, 15.71886984736413417, 96.68563167572563088 ) ) ;
#8883 = VERTEX_POINT ( 'NONE', #11825 ) ;
#8884 = AXIS2_PLACEMENT_3D ( 'NONE', #1439, #10129, #4350 ) ;
#8885 = DIRECTION ( 'NONE',  ( 1.000000000000000000, 0.000000000000000000, 0.000000000000000000 ) ) ;
#8886 = FACE_BOUND ( 'NONE', #7495, .T. ) ;
#8887 = ORIENTED_EDGE ( 'NONE', *, *, #9449, .F. ) ;
#8888 = CARTESIAN_POINT ( 'NONE',  ( 38.99999999999998579, 20.00000000000000355, 83.29316153445364534 ) ) ;
#8889 = EDGE_LOOP ( 'NONE', ( #2502, #10097, #1860, #11243 ) ) ;
#8890 = VECTOR ( 'NONE', #7477, 1000.000000000000000 ) ;
#8891 = CARTESIAN_POINT ( 'NONE',  ( -1.615502922434717492, 54.74315837822297937, -24.94959493428010688 ) ) ;
#8892 = CARTESIAN_POINT ( 'NONE',  ( 5.297557166928031691, 11.51226837079426524, -27.49566921010548270 ) ) ;
#8893 = CIRCLE ( 'NONE', #5451, 7.500000000000000000 ) ;
#8894 = CARTESIAN_POINT ( 'NONE',  ( 40.77500000054622120, 17.63344945572770328, 83.50966788445364841 ) ) ;
#8895 = CYLINDRICAL_SURFACE ( 'NONE', #11809, 7.499999999999978684 ) ;
#8896 = CARTESIAN_POINT ( 'NONE',  ( 49.27500000054622831, 27.65831843345427998, 90.79316153445363113 ) ) ;
#8897 = CARTESIAN_POINT ( 'NONE',  ( 45.39999999999999147, 27.13292387221364876, 88.47553407664153724 ) ) ;
#8898 = CARTESIAN_POINT ( 'NONE',  ( -9.466558637120989772, 23.23925856829589520, -23.13860710034107626 ) ) ;
#8899 = EDGE_CURVE ( 'NONE', #3460, #8756, #6934, .T. ) ;
#8900 = CARTESIAN_POINT ( 'NONE',  ( -23.10660171779821326, 12.50000000000000888, 140.6066017177982133 ) ) ;
#8901 = ORIENTED_EDGE ( 'NONE', *, *, #5690, .T. ) ;
#8902 = CARTESIAN_POINT ( 'NONE',  ( 30.65000000109246514, 20.00000000000000355, 83.29316153445364534 ) ) ;
#8903 = CARTESIAN_POINT ( 'NONE',  ( 3.061616998149962604E-15, 10.00000000000000000, 25.00000000000000000 ) ) ;
#8904 = VERTEX_POINT ( 'NONE', #7063 ) ;
#8905 = AXIS2_PLACEMENT_3D ( 'NONE', #2490, #1546, #596 ) ;
#8906 = VERTEX_POINT ( 'NONE', #1925 ) ;
#8907 = CARTESIAN_POINT ( 'NONE',  ( 0.000000000000000000, 0.000000000000000000, 169.9999999999999716 ) ) ;
#8908 = FACE_OUTER_BOUND ( 'NONE', #8574, .T. ) ;
#8909 = FACE_OUTER_BOUND ( 'NONE', #6964, .T. ) ;
#8910 = CARTESIAN_POINT ( 'NONE',  ( 29.17500000054623044, 26.92701409722686634, 88.54243821818162985 ) ) ;
#8911 = CARTESIAN_POINT ( 'NONE',  ( 29.07500000054622191, 24.28113015263587471, 84.90069139318163138 ) ) ;
#8912 = LINE ( 'NONE', #7010, #1129 ) ;
#8913 = CARTESIAN_POINT ( 'NONE',  ( -9.917191296150036806, 21.32702561569567834, 18.51082767248323080 ) ) ;
#8914 = CARTESIAN_POINT ( 'NONE',  ( -111.8465843842649292, 69.50000000000000000, 146.8533255156881978 ) ) ;
#8915 = ORIENTED_EDGE ( 'NONE', *, *, #10132, .T. ) ;
#8916 = CARTESIAN_POINT ( 'NONE',  ( 48.97500000054621694, 22.36655054427230382, 83.50966788445364841 ) ) ;
#8917 = CARTESIAN_POINT ( 'NONE',  ( 4.967652032308136789, 50.65502714036492904, -24.50156428836015721 ) ) ;
#8918 = CARTESIAN_POINT ( 'NONE',  ( -2.000000000000015543, 20.00000000000000355, 83.29316153445364534 ) ) ;
#8919 = VERTEX_POINT ( 'NONE', #227 ) ;
#8920 = DIRECTION ( 'NONE',  ( 0.000000000000000000, 0.000000000000000000, -1.000000000000000000 ) ) ;
#8921 = VECTOR ( 'NONE', #10051, 1000.000000000000000 ) ;
#8922 = ADVANCED_FACE ( 'NONE', ( #3134 ), #8840, .F. ) ;
#8923 = ORIENTED_EDGE ( 'NONE', *, *, #302, .T. ) ;
#8924 = CARTESIAN_POINT ( 'NONE',  ( 0.000000000000000000, -3.000000000000003109, 25.00000000000000355 ) ) ;
#8925 = CARTESIAN_POINT ( 'NONE',  ( -5.017800233121429088, 11.34386344135788605, -24.49301625034288321 ) ) ;
#8926 =( BOUNDED_CURVE ( )  B_SPLINE_CURVE ( 2, ( #8291, #4539, #1567, #5250, #7458, #492, #7394, #9121, #3466, #6442, #5439 ),
 .UNSPECIFIED., .F., .F. ) 
 B_SPLINE_CURVE_WITH_KNOTS ( ( 3, 2, 2, 2, 2, 3 ),
 ( 0.6666666666666666297, 0.6733333333333333393, 0.6800000000000000488, 0.6866666666666666474, 0.6933333333333333570, 0.6999999999999999556 ),
 .UNSPECIFIED. ) 
 CURVE ( )  GEOMETRIC_REPRESENTATION_ITEM ( )  RATIONAL_B_SPLINE_CURVE ( ( 1.000000000000000000, 0.9510565162951535312, 1.000000000000000000, 0.9510565162951535312, 1.000000000000000000, 0.9510565162951535312, 1.000000000000000000, 0.9510565162951535312, 1.000000000000000000, 0.9510565162951535312, 1.000000000000000000 ) ) 
 REPRESENTATION_ITEM ( '' )  );
#8927 = CARTESIAN_POINT ( 'NONE',  ( -5.000000000000004441, 40.00000000000000000, 69.99999999999998579 ) ) ;
#8928 = EDGE_CURVE ( 'NONE', #6723, #12336, #1379, .T. ) ;
#8929 = VECTOR ( 'NONE', #3727, 1000.000000000000114 ) ;
#8930 = DIRECTION ( 'NONE',  ( -1.000000000000000000, 0.000000000000000000, 0.000000000000000000 ) ) ;
#8931 = PRODUCT_DEFINITION_SHAPE ( 'NONE', 'NONE',  #12551 ) ;
#8932 = CARTESIAN_POINT ( 'NONE',  ( 9.408430673389327481, 23.42179483032959197, 97.48547108980501719 ) ) ;
#8933 = DIRECTION ( 'NONE',  ( -0.000000000000000000, -1.000000000000000000, -0.000000000000000000 ) ) ;
#8934 = CARTESIAN_POINT ( 'NONE',  ( -4.245899883333350111, 47.35448134532762055, -24.63697916171703994 ) ) ;
#8935 = CARTESIAN_POINT ( 'NONE',  ( 3.429011039554510417E-15, 10.00000000000000000, 28.00000000000000355 ) ) ;
#8936 = EDGE_CURVE ( 'NONE', #11306, #1221, #5805, .T. ) ;
#8937 = CARTESIAN_POINT ( 'NONE',  ( -3.767190843690196633, 46.69628320461708171, 27.74639135108192534 ) ) ;
#8938 = CARTESIAN_POINT ( 'NONE',  ( 43.67500000054621978, 22.36655054427230027, 98.07665518445361386 ) ) ;
#8939 = CARTESIAN_POINT ( 'NONE',  ( 3.763916608749744874, 46.69265501667148044, 20.66125156366808113 ) ) ;
#8940 = EDGE_LOOP ( 'NONE', ( #2047, #11369, #10752, #5418 ) ) ;
#8941 = EDGE_CURVE ( 'NONE', #5684, #6721, #3997, .T. ) ;
#8942 = AXIS2_PLACEMENT_3D ( 'NONE', #4440, #6287, #8193 ) ;
#8943 = CARTESIAN_POINT ( 'NONE',  ( -3.767201726441450571, 53.30370413573731980, 24.71563014075751141 ) ) ;
#8944 = EDGE_CURVE ( 'NONE', #7043, #5910, #10477, .T. ) ;
#8945 = CARTESIAN_POINT ( 'NONE',  ( 23.67500000054622333, 24.28113015263587116, 96.68563167572563088 ) ) ;
#8946 = CARTESIAN_POINT ( 'NONE',  ( 24.45000000109246585, 15.59161060780646046, 84.72553407664153724 ) ) ;
#8947 = EDGE_CURVE ( 'NONE', #9642, #4145, #7242, .T. ) ;
#8948 = CARTESIAN_POINT ( 'NONE',  ( 30.77500000054622831, 20.00000000000000355, 83.50966788445364841 ) ) ;
#8949 = CARTESIAN_POINT ( 'NONE',  ( 23.27500000054622475, 26.92701409722686634, 88.54243821818162985 ) ) ;
#8950 = CARTESIAN_POINT ( 'NONE',  ( 21.69999999999998508, 26.37988106264029398, 95.42841645007781892 ) ) ;
#8951 = CARTESIAN_POINT ( 'NONE',  ( 49.19999999999998863, 24.40838939219355197, 84.72553407664153724 ) ) ;
#8952 = CARTESIAN_POINT ( 'NONE',  ( 24.27500000054622475, 12.34168156654572535, 90.79316153445363113 ) ) ;
#8953 = VERTEX_POINT ( 'NONE', #2431 ) ;
#8954 = CARTESIAN_POINT ( 'NONE',  ( 5.000000000000000000, 4.685197434473814759, -5.637851296924623057E-15 ) ) ;
#8955 = ORIENTED_EDGE ( 'NONE', *, *, #2881, .F. ) ;
#8956 = DIRECTION ( 'NONE',  ( 0.000000000000000000, 0.000000000000000000, 1.000000000000000000 ) ) ;
#8957 = ORIENTED_EDGE ( 'NONE', *, *, #10705, .F. ) ;
#8958 = CARTESIAN_POINT ( 'NONE',  ( 53.00000000000000711, 20.00000000000000711, 189.9999999999999716 ) ) ;
#8959 = CARTESIAN_POINT ( 'NONE',  ( 41.27500000054622120, 26.92701409722686634, 88.54243821818162985 ) ) ;
#8960 = CARTESIAN_POINT ( 'NONE',  ( -10.00000000000000355, 20.00000000000000355, 109.9999999999999858 ) ) ;
#8961 = CARTESIAN_POINT ( 'NONE',  ( -3.975875746111922293, 46.95063182920211631, -27.71688932856698884 ) ) ;
#8962 = CARTESIAN_POINT ( 'NONE',  ( 38.97500000054623115, 22.36655054427230382, 83.50966788445364841 ) ) ;
#8963 = CARTESIAN_POINT ( 'NONE',  ( 39.39999999999999147, 27.13292387221364876, 88.47553407664153724 ) ) ;
#8964 = CARTESIAN_POINT ( 'NONE',  ( 46.37500000054622973, 13.07298590277314432, 88.54243821818161564 ) ) ;
#8965 = EDGE_LOOP ( 'NONE', ( #10463, #10063, #12170, #559 ) ) ;
#8966 = CARTESIAN_POINT ( 'NONE',  ( 33.35000000109246798, 26.37988106264029398, 95.42841645007781892 ) ) ;
#8967 = CARTESIAN_POINT ( 'NONE',  ( 2.286402882168606432, 10.25929110584701931, 24.89734643733720176 ) ) ;
#8968 = ORIENTED_EDGE ( 'NONE', *, *, #6919, .F. ) ;
#8969 = DIRECTION ( 'NONE',  ( 0.000000000000000000, 0.000000000000000000, -1.000000000000000000 ) ) ;
#8970 = VERTEX_POINT ( 'NONE', #1429 ) ;
#8971 = EDGE_CURVE ( 'NONE', #2108, #12320, #9280, .T. ) ;
#8972 = DIRECTION ( 'NONE',  ( 0.000000000000000000, 0.000000000000000000, -1.000000000000000000 ) ) ;
#8973 = CARTESIAN_POINT ( 'NONE',  ( -1.615502922434717492, 54.74315837822297937, -24.94959493428010688 ) ) ;
#8974 = ADVANCED_FACE ( 'NONE', ( #473 ), #11188, .T. ) ;
#8975 = DIRECTION ( 'NONE',  ( -0.000000000000000000, -1.000000000000000000, -0.000000000000000000 ) ) ;
#8976 = CARTESIAN_POINT ( 'NONE',  ( 29.07500000054623257, 26.19570976099943493, 86.29171490190961435 ) ) ;
#8977 = CARTESIAN_POINT ( 'NONE',  ( 30.47500000054622404, 13.07298590277314432, 88.54243821818161564 ) ) ;
#8978 = CIRCLE ( 'NONE', #10193, 6.000000000000000888 ) ;
#8979 = CARTESIAN_POINT ( 'NONE',  ( 39.65000000109246514, 20.00000000000000355, 98.29316153445363113 ) ) ;
#8980 = CARTESIAN_POINT ( 'NONE',  ( -0.6610962637957030763, 29.98365020075052811, 20.99219928172843197 ) ) ;
#8981 = CARTESIAN_POINT ( 'NONE',  ( 34.45000000109246940, 15.59161060780646046, 84.72553407664153724 ) ) ;
#8982 = ORIENTED_EDGE ( 'NONE', *, *, #8159, .T. ) ;
#8983 = CARTESIAN_POINT ( 'NONE',  ( 49.57500000054621836, 26.19570976099943849, 95.29460816699764791 ) ) ;
#8984 = CARTESIAN_POINT ( 'NONE',  ( 48.05000000109247082, 12.86707612778636012, 93.11078899226572503 ) ) ;
#8985 = ORIENTED_EDGE ( 'NONE', *, *, #9066, .F. ) ;
#8986 = LINE ( 'NONE', #3215, #1345 ) ;
#8987 = VERTEX_POINT ( 'NONE', #8274 ) ;
#8988 = CARTESIAN_POINT ( 'NONE',  ( -2.623156034030268202, 10.34458332881492559, -20.83793945939456549 ) ) ;
#8989 = AXIS2_PLACEMENT_3D ( 'NONE', #11458, #2765, #8480 ) ;
#8990 = CARTESIAN_POINT ( 'NONE',  ( 49.87500000054622262, 20.00000000000000355, 98.07665518445361386 ) ) ;
#8991 = B_SPLINE_CURVE_WITH_KNOTS ( 'NONE', 3,
 ( #9353, #8577, #12509, #9537, #10347, #10535, #4705, #3747, #9475, #6484, #716, #7502, #12323, #4520, #9415, #11372, #1664, #1725, #2801, #8395, #902, #10411, #5546, #4772, #7566, #10471, #2679, #9595 ),
 .UNSPECIFIED., .F., .F.,
 ( 4, 2, 2, 2, 2, 2, 2, 2, 2, 2, 2, 2, 2, 4 ),
 ( 0.04738924854463780201, 0.04936272659091893444, 0.05034946561405949372, 0.05133620463720005994, 0.05232294366034062616, 0.05330968268348119238, 0.05528316072976231788, 0.05626989975290288409, 0.05725663877604345031, 0.05923011682232458969, 0.06021685584546515591, 0.06120359486860571518, 0.06219033389174628140, 0.06317707291488684762 ),
 .UNSPECIFIED. ) ;
#8992 = CARTESIAN_POINT ( 'NONE',  ( -34.99999999999999289, 15.60660171779821681, 137.4999999999999716 ) ) ;
#8993 = EDGE_CURVE ( 'NONE', #5802, #10066, #10119, .T. ) ;
#8994 = CARTESIAN_POINT ( 'NONE',  ( 6.629859784148791846, 27.48642350972822612, 91.31199581522203346 ) ) ;
#8995 = CARTESIAN_POINT ( 'NONE',  ( -2.000000000000015543, 20.00000000000000355, 90.79316153445363113 ) ) ;
#8996 = AXIS2_PLACEMENT_3D ( 'NONE', #8276, #474, #1368 ) ;
#8997 = CARTESIAN_POINT ( 'NONE',  ( 5.315759107678847073, 28.47626550783180477, 20.31797234239212102 ) ) ;
#8998 = CARTESIAN_POINT ( 'NONE',  ( 1.500000000000001332, 0.000000000000000000, 0.000000000000000000 ) ) ;
#8999 = CARTESIAN_POINT ( 'NONE',  ( 6.615359460987012774, 27.52709606376180318, -19.93674538982958211 ) ) ;
#9000 = AXIS2_PLACEMENT_3D ( 'NONE', #1732, #6492, #10356 ) ;
#9001 = CARTESIAN_POINT ( 'NONE',  ( 44.47500000054622404, 13.80429023900056684, 86.29171490190961435 ) ) ;
#9002 = PRODUCT_DEFINITION_FORMATION_WITH_SPECIFIED_SOURCE ( 'ANY', '', #5993, .NOT_KNOWN. ) ;
#9003 = ADVANCED_FACE ( 'NONE', ( #9167 ), #3263, .F. ) ;
#9004 = CARTESIAN_POINT ( 'NONE',  ( 5.000000000000000000, 50.00000000000000000, 20.39607805437114152 ) ) ;
#9005 = VERTEX_POINT ( 'NONE', #7252 ) ;
#9006 =( BOUNDED_CURVE ( )  B_SPLINE_CURVE ( 2, ( #4927, #7594, #9690, #7530, #6571, #9564, #1937, #10565, #3711, #4735, #7721 ),
 .UNSPECIFIED., .F., .F. ) 
 B_SPLINE_CURVE_WITH_KNOTS ( ( 3, 2, 2, 2, 2, 3 ),
 ( 0.1000000000000000888, 0.1066666666666667151, 0.1133333333333333276, 0.1199999999999999678, 0.1266666666666665941, 0.1333333333333332205 ),
 .UNSPECIFIED. ) 
 CURVE ( )  GEOMETRIC_REPRESENTATION_ITEM ( )  RATIONAL_B_SPLINE_CURVE ( ( 0.9999999999999994449, 0.9510565162951540863, 1.000000000000000000, 0.9510565162951535312, 1.000000000000000000, 0.9510565162951535312, 1.000000000000000000, 0.9510565162951535312, 1.000000000000000000, 0.9510565162951543083, 0.9999999999999992228 ) ) 
 REPRESENTATION_ITEM ( '' )  );
#9007 = DIRECTION ( 'NONE',  ( -1.000000000000000000, 0.000000000000000000, 0.000000000000000000 ) ) ;
#9008 = AXIS2_PLACEMENT_3D ( 'NONE', #12042, #5255, #676 ) ;
#9009 = CARTESIAN_POINT ( 'NONE',  ( 46.59999999999998721, 12.86707612778636012, 88.47553407664152303 ) ) ;
#9010 = CARTESIAN_POINT ( 'NONE',  ( 44.07500000054622546, 15.71886984736413417, 96.68563167572563088 ) ) ;
#9011 = CARTESIAN_POINT ( 'NONE',  ( 32.97500000054622404, 24.28113015263587471, 84.90069139318163138 ) ) ;
#9012 = CARTESIAN_POINT ( 'NONE',  ( 23.07500000054622546, 24.28113015263587471, 84.90069139318163138 ) ) ;
#9013 = DIRECTION ( 'NONE',  ( -0.000000000000000000, 1.000000000000000000, 0.000000000000000000 ) ) ;
#9014 = PRESENTATION_STYLE_ASSIGNMENT (( #11798 ) ) ;
#9015 = CARTESIAN_POINT ( 'NONE',  ( 27.57500000054622902, 24.28113015263587116, 96.68563167572563088 ) ) ;
#9016 = ORIENTED_EDGE ( 'NONE', *, *, #930, .F. ) ;
#9017 = EDGE_CURVE ( 'NONE', #3374, #5229, #260, .T. ) ;
#9018 = CARTESIAN_POINT ( 'NONE',  ( 23.65000000109246514, 20.00000000000000355, 98.29316153445363113 ) ) ;
#9019 = ORIENTED_EDGE ( 'NONE', *, *, #243, .T. ) ;
#9020 = ORIENTED_EDGE ( 'NONE', *, *, #7484, .T. ) ;
#9021 = AXIS2_PLACEMENT_3D ( 'NONE', #11433, #2744, #207 ) ;
#9022 = DIRECTION ( 'NONE',  ( -1.000000000000000000, 0.000000000000000000, 0.000000000000000000 ) ) ;
#9023 = ORIENTED_EDGE ( 'NONE', *, *, #8654, .F. ) ;
#9024 = CARTESIAN_POINT ( 'NONE',  ( 6.000000000000000000, 2.919948986426526005, -5.057500000000003659 ) ) ;
#9025 = EDGE_CURVE ( 'NONE', #8335, #10986, #6233, .T. ) ;
#9026 = CARTESIAN_POINT ( 'NONE',  ( 37.67500000054621978, 24.28113015263587116, 96.68563167572563088 ) ) ;
#9027 = FACE_OUTER_BOUND ( 'NONE', #2381, .T. ) ;
#9028 = CARTESIAN_POINT ( 'NONE',  ( 26.99999999999998934, 20.00000000000000355, 83.29316153445364534 ) ) ;
#9029 = CARTESIAN_POINT ( 'NONE',  ( 39.47500000054622404, 26.92701409722686634, 93.04388485072563242 ) ) ;
#9030 = CARTESIAN_POINT ( 'NONE',  ( 43.39999999999998437, 27.13292387221364876, 88.47553407664153724 ) ) ;
#9031 = CIRCLE ( 'NONE', #3549, 10.00000000000000355 ) ;
#9032 = CARTESIAN_POINT ( 'NONE',  ( 45.67500000054621978, 22.36655054427230027, 98.07665518445361386 ) ) ;
#9033 = EDGE_LOOP ( 'NONE', ( #1814, #12356, #452, #10750, #11063 ) ) ;
#9034 = CARTESIAN_POINT ( 'NONE',  ( 24.35000000109246798, 13.62011893735971135, 86.15790661882942914 ) ) ;
#9035 = CARTESIAN_POINT ( 'NONE',  ( 6.000000000000000000, -2.919948986426525117, 5.057500000000004547 ) ) ;
#9036 = ORIENTED_EDGE ( 'NONE', *, *, #9336, .T. ) ;
#9037 = CARTESIAN_POINT ( 'NONE',  ( -1.648736202249158733, 29.86860657404073294, 27.95327759174768190 ) ) ;
#9038 = VECTOR ( 'NONE', #5133, 1000.000000000000000 ) ;
#9039 = VERTEX_POINT ( 'NONE', #3383 ) ;
#9040 = CARTESIAN_POINT ( 'NONE',  ( 24.65000000109246514, 20.00000000000000355, 83.29316153445364534 ) ) ;
#9041 = PRODUCT ( 'Support Axle', 'Support Axle', '', ( #1147 ) ) ;
#9042 = CARTESIAN_POINT ( 'NONE',  ( 6.000000000000000000, 8.759846959279592227, -5.057500000000009877 ) ) ;
#9043 = CARTESIAN_POINT ( 'NONE',  ( 48.49999999999998579, 12.11403331821300533, 90.79316153445363113 ) ) ;
#9044 = PRODUCT_DEFINITION_CONTEXT ( 'detailed design', #5461, 'design' ) ;
#9045 = CARTESIAN_POINT ( 'NONE',  ( 32.67500000054622689, 17.63344945572770328, 83.50966788445364841 ) ) ;
#9046 = CARTESIAN_POINT ( 'NONE',  ( 30.37500000054622618, 12.34168156654572535, 90.79316153445363113 ) ) ;
#9047 = CARTESIAN_POINT ( 'NONE',  ( 5.000000000000000000, 50.00000000000000000, 20.39607805437114152 ) ) ;
#9048 = DIRECTION ( 'NONE',  ( 1.000000000000000000, -0.000000000000000000, -0.000000000000000000 ) ) ;
#9049 = EDGE_LOOP ( 'NONE', ( #5661, #3657, #1780, #3564 ) ) ;
#9050 = CARTESIAN_POINT ( 'NONE',  ( 42.35000000109246798, 13.62011893735971135, 86.15790661882942914 ) ) ;
#9051 = LINE ( 'NONE', #11135, #10106 ) ;
#9052 = ORIENTED_EDGE ( 'NONE', *, *, #6526, .T. ) ;
#9053 = EDGE_CURVE ( 'NONE', #9486, #1716, #11125, .T. ) ;
#9054 = DIRECTION ( 'NONE',  ( 0.7071067811865489050, -0.000000000000000000, 0.7071067811865460184 ) ) ;
#9055 = ORIENTED_EDGE ( 'NONE', *, *, #7383, .F. ) ;
#9056 = FACE_OUTER_BOUND ( 'NONE', #8788, .T. ) ;
#9057 = AXIS2_PLACEMENT_3D ( 'NONE', #11153, #6395, #1512 ) ;
#9058 = CARTESIAN_POINT ( 'NONE',  ( 9.673501139021151829, 17.38172013086462542, -23.05305332146628317 ) ) ;
#9059 = CARTESIAN_POINT ( 'NONE',  ( 89.17200000000001125, 6.123233995736768255E-16, -5.000000000000001776 ) ) ;
#9060 = PLANE ( 'NONE',  #12106 ) ;
#9061 = CARTESIAN_POINT ( 'NONE',  ( 37.95000000109246940, 13.62011893735970958, 95.42841645007781892 ) ) ;
#9062 = CARTESIAN_POINT ( 'NONE',  ( 22.59999999999998721, 12.86707612778636012, 88.47553407664152303 ) ) ;
#9063 = PLANE ( 'NONE',  #9221 ) ;
#9064 = CARTESIAN_POINT ( 'NONE',  ( -1.299587538611466586, 54.83916993575238052, 20.96219696135102595 ) ) ;
#9065=STYLED_ITEM('',(#12591),#10428);
#9066 = EDGE_CURVE ( 'NONE', #438, #9553, #12205, .T. ) ;
#9067 = LINE ( 'NONE', #10829, #5790 ) ;
#9068 = CARTESIAN_POINT ( 'NONE',  ( -3.766911610146119305, 46.69571375074811925, -24.71569286637712892 ) ) ;
#9069 = ORIENTED_EDGE ( 'NONE', *, *, #854, .T. ) ;
#9070 = CARTESIAN_POINT ( 'NONE',  ( -5.000000000000000000, 50.00000000000000000, 24.49489742783178414 ) ) ;
#9071 = EDGE_CURVE ( 'NONE', #12540, #8162, #597, .T. ) ;
#9072 = AXIS2_PLACEMENT_3D ( 'NONE', #6242, #1485, #535 ) ;
#9073 = CARTESIAN_POINT ( 'NONE',  ( 28.29999999999998650, 13.62011893735970958, 95.42841645007781892 ) ) ;
#9074 = CARTESIAN_POINT ( 'NONE',  ( 45.57500000054621836, 26.19570976099943493, 95.29460816699764791 ) ) ;
#9075 = CARTESIAN_POINT ( 'NONE',  ( 30.47500000054622404, 13.80429023900056684, 86.29171490190961435 ) ) ;
#9076 = CARTESIAN_POINT ( 'NONE',  ( 7.061376757456052644, 12.91846277011745592, 93.27565706701507509 ) ) ;
#9077 = DIRECTION ( 'NONE',  ( -0.000000000000000000, -1.000000000000000000, -0.000000000000000000 ) ) ;
#9078 = CARTESIAN_POINT ( 'NONE',  ( 20.27158385259951956, 18.00000000000000355, 170.0000119999999697 ) ) ;
#9079 = CARTESIAN_POINT ( 'NONE',  ( 25.77500000054622831, 20.00000000000000355, 98.07665518445361386 ) ) ;
#9080 = ORIENTED_EDGE ( 'NONE', *, *, #6506, .T. ) ;
#9081 = CARTESIAN_POINT ( 'NONE',  ( -6.999999999999999112, 92.00000000000000000, 166.8533255156881694 ) ) ;
#9082 = ORIENTED_EDGE ( 'NONE', *, *, #10377, .F. ) ;
#9083 = EDGE_LOOP ( 'NONE', ( #3132, #9567, #2441, #1825, #11150 ) ) ;
#9084 = CARTESIAN_POINT ( 'NONE',  ( 38.49999999999999289, 12.11403331821300533, 90.79316153445363113 ) ) ;
#9085 = ORIENTED_EDGE ( 'NONE', *, *, #7341, .F. ) ;
#9086 = EDGE_CURVE ( 'NONE', #7706, #2249, #4621, .T. ) ;
#9087 = DIRECTION ( 'NONE',  ( 1.000000000000000000, 0.000000000000000000, 0.000000000000000000 ) ) ;
#9088 = VECTOR ( 'NONE', #5239, 1000.000000000000000 ) ;
#9089 = CARTESIAN_POINT ( 'NONE',  ( 40.57500000054621836, 13.80429023900056684, 86.29171490190961435 ) ) ;
#9090 = LINE ( 'NONE', #6292, #12417 ) ;
#9091 = EDGE_CURVE ( 'NONE', #8599, #11427, #11869, .T. ) ;
#9092 = CARTESIAN_POINT ( 'NONE',  ( -2.212795773503799523, 45.51331203296545169, -27.91280268202237025 ) ) ;
#9093 = CARTESIAN_POINT ( 'NONE',  ( 39.07500000054622546, 24.28113015263587471, 84.90069139318163138 ) ) ;
#9094 = CARTESIAN_POINT ( 'NONE',  ( 37.49999999999999289, 27.88596668178699645, 90.79316153445363113 ) ) ;
#9095 = CARTESIAN_POINT ( 'NONE',  ( 43.67500000054621978, 22.36655054427230027, 98.07665518445361386 ) ) ;
#9096 = ORIENTED_EDGE ( 'NONE', *, *, #12046, .F. ) ;
#9097 = CARTESIAN_POINT ( 'NONE',  ( 26.55000000109246017, 17.56310227825321135, 83.29316153445363113 ) ) ;
#9098 = DIRECTION ( 'NONE',  ( -0.7071067811865331398, 8.659560562355109119E-17, -0.7071067811865617836 ) ) ;
#9099 = ORIENTED_EDGE ( 'NONE', *, *, #1791, .T. ) ;
#9100 = EDGE_CURVE ( 'NONE', #1088, #10690, #5730, .T. ) ;
#9101 = CIRCLE ( 'NONE', #3609, 28.00000000000000000 ) ;
#9102 = CYLINDRICAL_SURFACE ( 'NONE', #11572, 7.499999999999992895 ) ;
#9103 = ORIENTED_EDGE ( 'NONE', *, *, #6303, .T. ) ;
#9104 = CARTESIAN_POINT ( 'NONE',  ( 4.147660976662388421, 10.89487115550369900, 27.69276736765331748 ) ) ;
#9105 = CARTESIAN_POINT ( 'NONE',  ( 4.839017051182398887, 48.69964289075914365, -27.57876268693809507 ) ) ;
#9106 = CARTESIAN_POINT ( 'NONE',  ( -50.00000000000001421, 0.000000000000000000, 169.9999999999999716 ) ) ;
#9107 = CIRCLE ( 'NONE', #8688, 23.49999999999999289 ) ;
#9108 = CARTESIAN_POINT ( 'NONE',  ( 28.67500000054623044, 17.63344945572770328, 83.50966788445364841 ) ) ;
#9109 = CARTESIAN_POINT ( 'NONE',  ( 25.67500000054622333, 24.28113015263587116, 96.68563167572563088 ) ) ;
#9110 = CARTESIAN_POINT ( 'NONE',  ( 6.000000000000000000, -2.919948986426525117, 5.057500000000004547 ) ) ;
#9111 = CLOSED_SHELL ( 'NONE', ( #2716, #343, #5839, #11720, #7544, #9315, #546, #9382, #12380, #11846, #2865, #3346, #8974, #8415, #2576, #5245, #11947, #1880, #86, #7303, #3923, #6994 ) ) ;
#9112 = DIRECTION ( 'NONE',  ( 0.000000000000000000, -1.000000000000000000, 1.039664082171044875E-15 ) ) ;
#9113 = ORIENTED_EDGE ( 'NONE', *, *, #6078, .T. ) ;
#9114 = CARTESIAN_POINT ( 'NONE',  ( 45.45000000109246230, 24.40838939219354842, 96.86078899226572503 ) ) ;
#9115 = DIRECTION ( 'NONE',  ( -1.000000000000000000, -0.000000000000000000, -0.000000000000000000 ) ) ;
#9116 = ORIENTED_EDGE ( 'NONE', *, *, #697, .F. ) ;
#9117 = DIRECTION ( 'NONE',  ( 0.000000000000000000, 0.000000000000000000, -1.000000000000000000 ) ) ;
#9118 = VERTEX_POINT ( 'NONE', #4646 ) ;
#9119 = DIRECTION ( 'NONE',  ( 1.000000000000000000, 0.000000000000000000, 0.000000000000000000 ) ) ;
#9120 = CARTESIAN_POINT ( 'NONE',  ( -8.961327849752377617, 24.44988401922752530, 23.33927995079777062 ) ) ;
#9121 = CARTESIAN_POINT ( 'NONE',  ( 29.29999999999998650, 26.37988106264029398, 86.15790661882942914 ) ) ;
#9122 = CARTESIAN_POINT ( 'NONE',  ( 37.65000000109246514, 20.00000000000000355, 98.29316153445363113 ) ) ;
#9123 = LINE ( 'NONE', #6263, #4629 ) ;
#9124 =( BOUNDED_CURVE ( )  B_SPLINE_CURVE ( 2, ( #9253, #5508, #5444, #4543, #7274, #434, #554, #10196, #8297, #10309, #6389 ),
 .UNSPECIFIED., .F., .F. ) 
 B_SPLINE_CURVE_WITH_KNOTS ( ( 3, 2, 2, 2, 2, 3 ),
 ( 0.2333333333333333093, 0.2399999999999999634, 0.2466666666666666452, 0.2533333333333333548, 0.2600000000000000089, 0.2666666666666666630 ),
 .UNSPECIFIED. ) 
 CURVE ( )  GEOMETRIC_REPRESENTATION_ITEM ( )  RATIONAL_B_SPLINE_CURVE ( ( 1.000000000000000222, 0.9510565162951533091, 1.000000000000000000, 0.9510565162951535312, 1.000000000000000000, 0.9510565162951535312, 1.000000000000000000, 0.9510565162951535312, 1.000000000000000000, 0.9510565162951535312, 1.000000000000000000 ) ) 
 REPRESENTATION_ITEM ( '' )  );
#9125 = AXIS2_PLACEMENT_3D ( 'NONE', #3807, #11553, #137 ) ;
#9126 = CARTESIAN_POINT ( 'NONE',  ( 0.000000000000000000, 0.000000000000000000, 0.000000000000000000 ) ) ;
#9127 = CARTESIAN_POINT ( 'NONE',  ( -8.654264301703824103, 14.97889801067282889, 26.62950408590382168 ) ) ;
#9128 = DIRECTION ( 'NONE',  ( 0.000000000000000000, 0.000000000000000000, 1.000000000000000000 ) ) ;
#9129 = LINE ( 'NONE', #5259, #8517 ) ;
#9130 = ORIENTED_EDGE ( 'NONE', *, *, #11106, .T. ) ;
#9131 = B_SPLINE_CURVE_WITH_KNOTS ( 'NONE', 3,
 ( #8474, #795, #5688, #4666, #1741, #6565, #7587, #5623, #9494, #1865, #11511, #2823, #1680, #11389, #6687, #8658, #5746, #4854, #10556, #9617, #925, #10367, #10613, #11452, #7710, #8535, #10430, #2699 ),
 .UNSPECIFIED., .F., .F.,
 ( 4, 2, 2, 2, 2, 2, 2, 2, 2, 2, 2, 2, 2, 4 ),
 ( 0.03159723681526421801, 0.03258403062298791120, 0.03357082443071160438, 0.03554441204615898381, 0.03653120585388267699, 0.03751799966160637018, 0.03850479346933006336, 0.03949158727705375654, 0.04146517489250114985, 0.04245196870022484303, 0.04343876250794853622, 0.04541235012339592259, 0.04639914393111962271, 0.04738593773884331589 ),
 .UNSPECIFIED. ) ;
#9132 = CARTESIAN_POINT ( 'NONE',  ( -7.523754161084773351, 13.40468021027817791, -26.97107581164716095 ) ) ;
#9133 = AXIS2_PLACEMENT_3D ( 'NONE', #2646, #3530, #7467 ) ;
#9134 = CARTESIAN_POINT ( 'NONE',  ( 4.142194555499470354, 10.89240068329948130, -27.69358117727547963 ) ) ;
#9135 = ADVANCED_FACE ( 'NONE', ( #4707 ), #1666, .F. ) ;
#9136 = CARTESIAN_POINT ( 'NONE',  ( 28.39999999999998792, 12.86707612778636012, 93.11078899226572503 ) ) ;
#9137 = CARTESIAN_POINT ( 'NONE',  ( 42.77500000054622831, 17.63344945572770328, 83.50966788445364841 ) ) ;
#9138 = CARTESIAN_POINT ( 'NONE',  ( 24.67500000054622689, 17.63344945572770328, 83.50966788445364841 ) ) ;
#9139 = CARTESIAN_POINT ( 'NONE',  ( 3.061617023331388775E-15, 45.00000000000000711, 25.00000000000000000 ) ) ;
#9140 = CARTESIAN_POINT ( 'NONE',  ( 3.429011037612589670E-15, 0.000000000000000000, 28.00000000000000355 ) ) ;
#9141 = CARTESIAN_POINT ( 'NONE',  ( 35.49999999999998579, 27.88596668178699645, 90.79316153445363113 ) ) ;
#9142 = DIRECTION ( 'NONE',  ( 0.000000000000000000, -0.4999999999999985012, 0.8660254037844394848 ) ) ;
#9143 = CARTESIAN_POINT ( 'NONE',  ( 27.17500000054622689, 26.92701409722686634, 88.54243821818162985 ) ) ;
#9144 = ORIENTED_EDGE ( 'NONE', *, *, #919, .F. ) ;
#9145 = AXIS2_PLACEMENT_3D ( 'NONE', #7248, #8148, #11121 ) ;
#9146 = PRODUCT_DEFINITION_SHAPE ( 'NONE', 'NONE',  #771 ) ;
#9147 = CARTESIAN_POINT ( 'NONE',  ( 33.35000000109246088, 26.37988106264029398, 95.42841645007781892 ) ) ;
#9148 = VERTEX_POINT ( 'NONE', #10290 ) ;
#9149 = PLANE ( 'NONE',  #6503 ) ;
#9150 = VERTEX_POINT ( 'NONE', #11375 ) ;
#9151 = AXIS2_PLACEMENT_3D ( 'NONE', #9973, #9022, #1762 ) ;
#9152 = CARTESIAN_POINT ( 'NONE',  ( 33.47500000054622404, 26.92701409722686634, 93.04388485072563242 ) ) ;
#9153 = DIRECTION ( 'NONE',  ( 0.000000000000000000, 0.5000000000000012212, 0.8660254037844379305 ) ) ;
#9154 = CARTESIAN_POINT ( 'NONE',  ( 42.87500000054622262, 22.36655054427230382, 83.50966788445364841 ) ) ;
#9155 = CARTESIAN_POINT ( 'NONE',  ( 31.57500000054622191, 26.19570976099943493, 95.29460816699764791 ) ) ;
#9156 = CARTESIAN_POINT ( 'NONE',  ( 38.69999999999998863, 13.62011893735971135, 86.15790661882942914 ) ) ;
#9157 = ADVANCED_FACE ( 'NONE', ( #7504 ), #10473, .F. ) ;
#9158 = CARTESIAN_POINT ( 'NONE',  ( 47.17500000054623399, 26.92701409722686634, 88.54243821818162985 ) ) ;
#9159 = VERTEX_POINT ( 'NONE', #11246 ) ;
#9160 = CARTESIAN_POINT ( 'NONE',  ( 24.25000000109246301, 12.86707612778636012, 88.47553407664152303 ) ) ;
#9161 = DIRECTION ( 'NONE',  ( 0.000000000000000000, 1.000000000000000000, -1.224646799147353207E-16 ) ) ;
#9162 = EDGE_LOOP ( 'NONE', ( #12109, #7327, #3018, #12089, #1178, #5940, #10720, #3184, #11185, #5924, #467, #10344, #11570, #2061, #4533, #11658 ) ) ;
#9163 = CARTESIAN_POINT ( 'NONE',  ( -4.458389208371986712, 28.97542069971310141, 27.64960765936604759 ) ) ;
#9164 = VERTEX_POINT ( 'NONE', #12450 ) ;
#9165 = CARTESIAN_POINT ( 'NONE',  ( -34.72841614740047333, 18.00000000000000355, 152.2284161474004520 ) ) ;
#9166 = CARTESIAN_POINT ( 'NONE',  ( 23.99529484836403626, 12.50000000000001066, 148.5047051516359318 ) ) ;
#9167 = FACE_OUTER_BOUND ( 'NONE', #8471, .T. ) ;
#9168 = CARTESIAN_POINT ( 'NONE',  ( 6.000000000000000000, 0.000000000000000000, 0.000000000000000000 ) ) ;
#9169 = CARTESIAN_POINT ( 'NONE',  ( 23.17500000054622689, 26.92701409722686634, 88.54243821818162985 ) ) ;
#9170 = CARTESIAN_POINT ( 'NONE',  ( 25.17500000054622689, 26.19570976099943493, 86.29171490190961435 ) ) ;
#9171 = EDGE_CURVE ( 'NONE', #6828, #1723, #5825, .T. ) ;
#9172 = CARTESIAN_POINT ( 'NONE',  ( 9.660534914401177176, 22.60440596647124067, 26.28087847349582518 ) ) ;
#9173 = CARTESIAN_POINT ( 'NONE',  ( 0.000000000000000000, -2.919948986426523341, 5.057500000000002771 ) ) ;
#9174 = ORIENTED_EDGE ( 'NONE', *, *, #737, .T. ) ;
#9175 = CARTESIAN_POINT ( 'NONE',  ( 42.45000000109246940, 15.59161060780646046, 84.72553407664153724 ) ) ;
#9176 = FILL_AREA_STYLE ('',( #11195 ) ) ;
#9177 = ORIENTED_EDGE ( 'NONE', *, *, #8798, .T. ) ;
#9178 = DIRECTION ( 'NONE',  ( 0.000000000000000000, 0.000000000000000000, 1.000000000000000000 ) ) ;
#9179 = EDGE_CURVE ( 'NONE', #2899, #2755, #3750, .T. ) ;
#9180 = VERTEX_POINT ( 'NONE', #2803 ) ;
#9181 = CARTESIAN_POINT ( 'NONE',  ( 0.6000000000000033085, 0.000000000000000000, 0.000000000000000000 ) ) ;
#9182 = CARTESIAN_POINT ( 'NONE',  ( 8.963427797786382101, 15.55435157282535741, -23.33847234685102379 ) ) ;
#9183 = CARTESIAN_POINT ( 'NONE',  ( -2.000000000000015543, 20.00000000000000355, 90.79316153445363113 ) ) ;
#9184 = AXIS2_PLACEMENT_3D ( 'NONE', #11813, #1973, #2169 ) ;
#9185 = ADVANCED_FACE ( 'NONE', ( #5605 ), #12326, .F. ) ;
#9186 = CARTESIAN_POINT ( 'NONE',  ( 10.00000000000000000, 0.000000000000000000, 0.000000000000000000 ) ) ;
#9187 = CARTESIAN_POINT ( 'NONE',  ( 0.000000000000000000, 18.00000000000000355, 169.9999999999999716 ) ) ;
#9188 = DIRECTION ( 'NONE',  ( 0.000000000000000000, 0.4999999999999987232, -0.8660254037844392627 ) ) ;
#9189 = FACE_OUTER_BOUND ( 'NONE', #3362, .T. ) ;
#9190 = DIRECTION ( 'NONE',  ( 1.000000000000000000, -0.000000000000000000, -0.000000000000000000 ) ) ;
#9191 = CARTESIAN_POINT ( 'NONE',  ( 1.313665803496629980, 29.93556061881280428, 24.97400592093060112 ) ) ;
#9192 = AXIS2_PLACEMENT_3D ( 'NONE', #9437, #12351, #3650 ) ;
#9193 = CARTESIAN_POINT ( 'NONE',  ( 4.967314895201458746, 49.34232189057839690, 20.40416878132349510 ) ) ;
#9194 = ORIENTED_EDGE ( 'NONE', *, *, #10302, .F. ) ;
#9195 = CARTESIAN_POINT ( 'NONE',  ( -5.000000000000000000, 50.32679387323496911, 24.49489742783177704 ) ) ;
#9196 = CARTESIAN_POINT ( 'NONE',  ( 34.72841614740047333, 18.00000000000000355, 169.9999999999999716 ) ) ;
#9197 = CARTESIAN_POINT ( 'NONE',  ( 27.99999999999998579, 20.00000000000000355, 98.29316153445363113 ) ) ;
#9198 = CARTESIAN_POINT ( 'NONE',  ( 44.27500000054622120, 13.07298590277314254, 93.04388485072563242 ) ) ;
#9199 = TOROIDAL_SURFACE ( 'NONE', #6165, 13.85889894354065355, 10.00000000000000000 ) ;
#9200 = CARTESIAN_POINT ( 'NONE',  ( 23.87500000054622618, 17.63344945572769973, 98.07665518445361386 ) ) ;
#9201 = CARTESIAN_POINT ( 'NONE',  ( 7.946724766127979400, 13.89530605390606688, -23.70643652970303350 ) ) ;
#9202 = PLANE ( 'NONE',  #10583 ) ;
#9203 = PRODUCT_DEFINITION_FORMATION_WITH_SPECIFIED_SOURCE ( 'ANY', '', #8127, .NOT_KNOWN. ) ;
#9204 = CARTESIAN_POINT ( 'NONE',  ( 31.79999999999998650, 24.40838939219354842, 96.86078899226572503 ) ) ;
#9205 = ORIENTED_EDGE ( 'NONE', *, *, #8621, .T. ) ;
#9206 = CARTESIAN_POINT ( 'NONE',  ( 6.000000000000000000, -4.379923479639794337, 2.528750000000004938 ) ) ;
#9207 = EDGE_LOOP ( 'NONE', ( #5803, #10158, #1423, #6048, #6161 ) ) ;
#9208 = EDGE_CURVE ( 'NONE', #4057, #10641, #7216, .T. ) ;
#9209 = DIRECTION ( 'NONE',  ( 0.000000000000000000, -1.000000000000000000, 0.000000000000000000 ) ) ;
#9210 = ORIENTED_EDGE ( 'NONE', *, *, #3813, .T. ) ;
#9211 = AXIS2_PLACEMENT_3D ( 'NONE', #1729, #1667, #2621 ) ;
#9212 = VECTOR ( 'NONE', #2591, 1000.000000000000114 ) ;
#9213 = CARTESIAN_POINT ( 'NONE',  ( 31.77500000054622831, 22.36655054427230027, 98.07665518445361386 ) ) ;
#9214 = DIRECTION ( 'NONE',  ( -0.000000000000000000, -1.000000000000000000, -0.000000000000000000 ) ) ;
#9215 = CARTESIAN_POINT ( 'NONE',  ( 45.67500000054621978, 22.36655054427230027, 98.07665518445361386 ) ) ;
#9216 = CARTESIAN_POINT ( 'NONE',  ( 35.87500000054622973, 20.00000000000000355, 98.07665518445361386 ) ) ;
#9217 = CARTESIAN_POINT ( 'NONE',  ( 39.09999999999999432, 22.43689772174679575, 83.29316153445363113 ) ) ;
#9218 = CARTESIAN_POINT ( 'NONE',  ( 3.547335893868845513, 29.35536450536750408, 24.74892486337281738 ) ) ;
#9219 = CARTESIAN_POINT ( 'NONE',  ( 42.87500000054622973, 22.36655054427230382, 83.50966788445364841 ) ) ;
#9220 = ORIENTED_EDGE ( 'NONE', *, *, #11960, .F. ) ;
#9221 = AXIS2_PLACEMENT_3D ( 'NONE', #11785, #10898, #7024 ) ;
#9222 = CARTESIAN_POINT ( 'NONE',  ( 24.75000000109246656, 22.43689772174679575, 83.29316153445363113 ) ) ;
#9223 = CARTESIAN_POINT ( 'NONE',  ( -0.3269774092232215490, 45.00000000000000000, 25.00000000000000711 ) ) ;
#9224 = VERTEX_POINT ( 'NONE', #6545 ) ;
#9225 = DIRECTION ( 'NONE',  ( 0.000000000000000000, 0.000000000000000000, -1.000000000000000000 ) ) ;
#9226 = ORIENTED_EDGE ( 'NONE', *, *, #5360, .T. ) ;
#9227 = CARTESIAN_POINT ( 'NONE',  ( 5.000000000000000000, 2.342598717236900718, -4.057500000000001883 ) ) ;
#9228 = DIRECTION ( 'NONE',  ( 0.000000000000000000, 0.000000000000000000, -1.000000000000000000 ) ) ;
#9229 = EDGE_CURVE ( 'NONE', #5525, #4126, #10895, .T. ) ;
#9230 = DIRECTION ( 'NONE',  ( -0.000000000000000000, -0.000000000000000000, -1.000000000000000000 ) ) ;
#9231 = CIRCLE ( 'NONE', #5784, 7.499999999999992895 ) ;
#9232 = DIRECTION ( 'NONE',  ( -1.000000000000000000, -0.000000000000000000, -0.000000000000000000 ) ) ;
#9233 = CARTESIAN_POINT ( 'NONE',  ( 22.17500000054622689, 13.07298590277314254, 93.04388485072563242 ) ) ;
#9234 = CARTESIAN_POINT ( 'NONE',  ( 23.47500000054622404, 26.92701409722686634, 93.04388485072563242 ) ) ;
#9235 = ADVANCED_FACE ( 'NONE', ( #1607, #10537 ), #9478, .T. ) ;
#9236 = FACE_OUTER_BOUND ( 'NONE', #7990, .T. ) ;
#9237 = CARTESIAN_POINT ( 'NONE',  ( 0.000000000000000000, 0.000000000000000000, -28.00000000000000355 ) ) ;
#9238 = ORIENTED_EDGE ( 'NONE', *, *, #498, .F. ) ;
#9239 = CARTESIAN_POINT ( 'NONE',  ( 41.45000000109246940, 24.40838939219354842, 96.86078899226572503 ) ) ;
#9240 = CARTESIAN_POINT ( 'NONE',  ( 4.743537283058001819, 51.61420199850529400, -24.54618281552716041 ) ) ;
#9241 = ORIENTED_EDGE ( 'NONE', *, *, #5764, .T. ) ;
#9242 = CARTESIAN_POINT ( 'NONE',  ( 47.19999999999998863, 24.40838939219355197, 84.72553407664153724 ) ) ;
#9243 = ORIENTED_EDGE ( 'NONE', *, *, #939, .T. ) ;
#9244 = AXIS2_PLACEMENT_3D ( 'NONE', #2961, #11397, #8668 ) ;
#9245 = CARTESIAN_POINT ( 'NONE',  ( -7.929079634139357680, 13.89786668772332767, -23.71027527960010417 ) ) ;
#9246 = CARTESIAN_POINT ( 'NONE',  ( -3.243418093453738216, 29.48203249043655561, 24.79625640031606082 ) ) ;
#9247 = CARTESIAN_POINT ( 'NONE',  ( -6.999999999999999112, 77.00000000000000000, 101.8533255156881978 ) ) ;
#9248 = CARTESIAN_POINT ( 'NONE',  ( 5.000000000000000000, 50.00000000000000000, 24.49489742783178059 ) ) ;
#9249 = ADVANCED_FACE ( 'NONE', ( #9356 ), #657, .T. ) ;
#9250 = VECTOR ( 'NONE', #2442, 1000.000000000000000 ) ;
#9251 = CARTESIAN_POINT ( 'NONE',  ( -8.967015720386880773, 15.56160195868188545, 23.33709189419391805 ) ) ;
#9252 = DIRECTION ( 'NONE',  ( 1.000000000000000000, 0.000000000000000000, 0.000000000000000000 ) ) ;
#9253 = CARTESIAN_POINT ( 'NONE',  ( 42.99999999999999289, 20.00000000000000355, 83.29316153445364534 ) ) ;
#9254 = CARTESIAN_POINT ( 'NONE',  ( 6.000000000000000000, -5.839897972853060892, 7.806255641895631925E-15 ) ) ;
#9255 = CARTESIAN_POINT ( 'NONE',  ( -50.00000000000001421, 40.00000000000000000, 132.8533255156884820 ) ) ;
#9256 = EDGE_CURVE ( 'NONE', #6052, #1748, #7775, .T. ) ;
#9257 = CARTESIAN_POINT ( 'NONE',  ( 46.95000000109246230, 26.37988106264029398, 86.15790661882942914 ) ) ;
#9258 = EDGE_LOOP ( 'NONE', ( #10174, #9737, #980, #9177, #1299, #3776 ) ) ;
#9259 = ADVANCED_FACE ( 'NONE', ( #10660 ), #3056, .F. ) ;
#9260 = EDGE_CURVE ( 'NONE', #7703, #730, #3201, .T. ) ;
#9261 = CARTESIAN_POINT ( 'NONE',  ( 49.99999999999998579, 20.00000000000000355, 83.29316153445363113 ) ) ;
#9262 = DIRECTION ( 'NONE',  ( -1.000000000000000000, -0.000000000000000000, -0.000000000000000000 ) ) ;
#9263 = CARTESIAN_POINT ( 'NONE',  ( 41.27500000054622120, 26.92701409722686634, 88.54243821818162985 ) ) ;
#9264 = AXIS2_PLACEMENT_3D ( 'NONE', #2208, #6833, #10822 ) ;
#9265 = CARTESIAN_POINT ( 'NONE',  ( 27.17500000054622689, 26.92701409722686634, 88.54243821818162985 ) ) ;
#9266 = CARTESIAN_POINT ( 'NONE',  ( 9.237585187503595918, 16.16340832531784244, 84.34413360981309893 ) ) ;
#9267 = CARTESIAN_POINT ( 'NONE',  ( 44.65000000109246514, 20.00000000000000355, 83.29316153445364534 ) ) ;
#9268 = CARTESIAN_POINT ( 'NONE',  ( 6.000000000000000000, -2.919948986426538440, -5.057499999999997442 ) ) ;
#9269 = PLANE ( 'NONE',  #6073 ) ;
#9270 = VERTEX_POINT ( 'NONE', #1971 ) ;
#9271 = CARTESIAN_POINT ( 'NONE',  ( 12.00000000000000355, 0.000000000000000000, 0.000000000000000000 ) ) ;
#9272 = VERTEX_POINT ( 'NONE', #10786 ) ;
#9273 = CARTESIAN_POINT ( 'NONE',  ( 2.562745747226488176E-15, 30.00000000000001066, 21.00000000000000000 ) ) ;
#9274 = CIRCLE ( 'NONE', #7848, 10.00000000000000178 ) ;
#9275 = CARTESIAN_POINT ( 'NONE',  ( 33.77500000054622831, 22.36655054427230027, 98.07665518445361386 ) ) ;
#9276 = CARTESIAN_POINT ( 'NONE',  ( -4.493244791708733032, 52.21758165739003488, -27.63741816232653647 ) ) ;
#9277 = CARTESIAN_POINT ( 'NONE',  ( 44.47500000054622404, 13.80429023900056684, 86.29171490190961435 ) ) ;
#9278 = CARTESIAN_POINT ( 'NONE',  ( 33.07500000054622546, 24.28113015263587471, 84.90069139318163138 ) ) ;
#9279 = CARTESIAN_POINT ( 'NONE',  ( 33.29999999999999005, 26.37988106264029398, 86.15790661882942914 ) ) ;
#9280 = CIRCLE ( 'NONE', #9072, 6.500000000000000888 ) ;
#9281 = CARTESIAN_POINT ( 'NONE',  ( 7.298955741910466699, 26.84326632351102759, 23.91197098918000918 ) ) ;
#9282 = CARTESIAN_POINT ( 'NONE',  ( 39.67500000054623399, 22.36655054427230027, 98.07665518445361386 ) ) ;
#9283 = ORIENTED_EDGE ( 'NONE', *, *, #5764, .F. ) ;
#9284 = CARTESIAN_POINT ( 'NONE',  ( 23.95000000109246585, 13.62011893735971135, 95.42841645007781892 ) ) ;
#9285 = DIRECTION ( 'NONE',  ( 0.000000000000000000, 1.224646799147351728E-16, 1.000000000000000000 ) ) ;
#9286 = EDGE_LOOP ( 'NONE', ( #6483, #2439, #5484, #4452 ) ) ;
#9287 = FACE_OUTER_BOUND ( 'NONE', #5832, .T. ) ;
#9288 = EDGE_LOOP ( 'NONE', ( #5103, #7340 ) ) ;
#9289 = DIRECTION ( 'NONE',  ( 0.000000000000000000, 0.000000000000000000, -1.000000000000000000 ) ) ;
#9290 = VECTOR ( 'NONE', #2560, 1000.000000000000000 ) ;
#9291 = DIRECTION ( 'NONE',  ( 1.000000000000000000, 0.000000000000000000, 0.000000000000000000 ) ) ;
#9292 = DIRECTION ( 'NONE',  ( -1.000000000000000000, -0.000000000000000000, -0.000000000000000000 ) ) ;
#9293 = LINE ( 'NONE', #1608, #1892 ) ;
#9294 = EDGE_CURVE ( 'NONE', #2160, #8662, #10595, .T. ) ;
#9295 = CARTESIAN_POINT ( 'NONE',  ( 21.87500000054622973, 17.63344945572769973, 98.07665518445361386 ) ) ;
#9296 = CARTESIAN_POINT ( 'NONE',  ( 22.97500000054622049, 22.36655054427230382, 83.50966788445364841 ) ) ;
#9297 = DIRECTION ( 'NONE',  ( 1.000000000000000000, -0.000000000000000000, -0.000000000000000000 ) ) ;
#9298 = CARTESIAN_POINT ( 'NONE',  ( 3.061617023331388775E-15, 45.00000000000000711, 25.00000000000000000 ) ) ;
#9299 = CIRCLE ( 'NONE', #3814, 10.00000000000000000 ) ;
#9300 = ORIENTED_EDGE ( 'NONE', *, *, #11734, .F. ) ;
#9301 = CARTESIAN_POINT ( 'NONE',  ( 46.15000000109246514, 12.11403331821300533, 90.79316153445363113 ) ) ;
#9302 = CARTESIAN_POINT ( 'NONE',  ( 4.493076325134499172, 52.21789521489533570, -24.59326131088672440 ) ) ;
#9303 = EDGE_LOOP ( 'NONE', ( #2564, #4422, #3244, #9756, #6632 ) ) ;
#9304 = FACE_OUTER_BOUND ( 'NONE', #532, .T. ) ;
#9305 = ORIENTED_EDGE ( 'NONE', *, *, #747, .F. ) ;
#9306 = DIRECTION ( 'NONE',  ( 0.000000000000000000, 0.000000000000000000, -1.000000000000000000 ) ) ;
#9307 = CARTESIAN_POINT ( 'NONE',  ( -8.483825669166648709, 25.30371668182424827, 23.51725424962153355 ) ) ;
#9308 = CIRCLE ( 'NONE', #11622, 0.5999999999999998668 ) ;
#9309 = DIRECTION ( 'NONE',  ( -0.000000000000000000, -1.000000000000000000, -0.000000000000000000 ) ) ;
#9310 = CLOSED_SHELL ( 'NONE', ( #4217, #6712, #8861, #1412, #11705, #9857, #5023, #10137, #1784, #5587, #11168, #797, #3627, #6042 ) ) ;
#9311 = VECTOR ( 'NONE', #6498, 1000.000000000000000 ) ;
#9312 = CARTESIAN_POINT ( 'NONE',  ( 4.967437465254620932, 50.65784153438875848, 24.50160996501502098 ) ) ;
#9313 = CARTESIAN_POINT ( 'NONE',  ( 38.15000000109245804, 12.11403331821300533, 90.79316153445363113 ) ) ;
#9314 = DIRECTION ( 'NONE',  ( -0.000000000000000000, -1.000000000000000000, -0.000000000000000000 ) ) ;
#9315 = ADVANCED_FACE ( 'NONE', ( #970 ), #4820, .T. ) ;
#9316 = ADVANCED_FACE ( 'NONE', ( #11559 ), #4002, .F. ) ;
#9317 = DIRECTION ( 'NONE',  ( -1.000000000000000000, 0.000000000000000000, 0.000000000000000000 ) ) ;
#9318 = CARTESIAN_POINT ( 'NONE',  ( 10.00000000000000888, 20.33378987232122981, 22.91287847477920536 ) ) ;
#9319 = AXIS2_PLACEMENT_3D ( 'NONE', #12485, #7543, #1703 ) ;
#9320 = CARTESIAN_POINT ( 'NONE',  ( -4.556215257066872582, 52.06578128350423640, 24.58139409886873139 ) ) ;
#9321 = ORIENTED_EDGE ( 'NONE', *, *, #11393, .F. ) ;
#9322 = TOROIDAL_SURFACE ( 'NONE', #3235, 13.85889894354065355, 10.00000000000000000 ) ;
#9323 = DIRECTION ( 'NONE',  ( -1.000000000000000000, -0.000000000000000000, -0.000000000000000000 ) ) ;
#9324 = CARTESIAN_POINT ( 'NONE',  ( 2.912936886510098855, 54.06713064528141643, 24.83009325023465763 ) ) ;
#9325 = CARTESIAN_POINT ( 'NONE',  ( 38.17500000054622689, 13.80429023900056507, 95.29460816699764791 ) ) ;
#9326 = CARTESIAN_POINT ( 'NONE',  ( 26.07500000054622546, 13.80429023900056507, 95.29460816699764791 ) ) ;
#9327 = CARTESIAN_POINT ( 'NONE',  ( 8.250161558006810836, 14.33538267060655436, 85.85517769022618495 ) ) ;
#9328 = CARTESIAN_POINT ( 'NONE',  ( 3.303926766530076442, 46.23304915065238418, 24.78181020466353601 ) ) ;
#9329 = EDGE_CURVE ( 'NONE', #2485, #2831, #8666, .T. ) ;
#9330 = DIRECTION ( 'NONE',  ( 0.000000000000000000, 0.000000000000000000, -1.000000000000000000 ) ) ;
#9331 = CARTESIAN_POINT ( 'NONE',  ( 6.000000000000000000, -2.919948986426523341, 5.057500000000002771 ) ) ;
#9332 = ORIENTED_EDGE ( 'NONE', *, *, #12502, .T. ) ;
#9333 = CARTESIAN_POINT ( 'NONE',  ( 10.00000000000003020, 20.00000000000000711, 162.0000000000000000 ) ) ;
#9334 = AXIS2_PLACEMENT_3D ( 'NONE', #2861, #9779, #4768 ) ;
#9335 = DIRECTION ( 'NONE',  ( -0.4999999999999892308, -0.000000000000000000, 0.8660254037844448138 ) ) ;
#9336 = EDGE_CURVE ( 'NONE', #5816, #4148, #3118, .T. ) ;
#9337 =( BOUNDED_CURVE ( )  B_SPLINE_CURVE ( 2, ( #1930, #9936, #11708, #3075, #2122, #6818, #167, #2955, #1243, #10682, #3013 ),
 .UNSPECIFIED., .F., .F. ) 
 B_SPLINE_CURVE_WITH_KNOTS ( ( 3, 2, 2, 2, 2, 3 ),
 ( 0.1666666666666665741, 0.1733333333333332560, 0.1799999999999999101, 0.1866666666666665919, 0.1933333333333332460, 0.1999999999999999278 ),
 .UNSPECIFIED. ) 
 CURVE ( )  GEOMETRIC_REPRESENTATION_ITEM ( )  RATIONAL_B_SPLINE_CURVE ( ( 1.000000000000000666, 0.9510565162951529761, 1.000000000000000000, 0.9510565162951535312, 1.000000000000000000, 0.9510565162951535312, 1.000000000000000000, 0.9510565162951535312, 1.000000000000000000, 0.9510565162951540863, 0.9999999999999994449 ) ) 
 REPRESENTATION_ITEM ( '' )  );
#9338 = CARTESIAN_POINT ( 'NONE',  ( 32.87500000054622262, 20.00000000000000355, 83.50966788445364841 ) ) ;
#9339 = CARTESIAN_POINT ( 'NONE',  ( 28.95000000109246585, 26.37988106264029398, 86.15790661882942914 ) ) ;
#9340 = CARTESIAN_POINT ( 'NONE',  ( 48.97500000054622404, 24.28113015263587471, 84.90069139318163138 ) ) ;
#9341 = CARTESIAN_POINT ( 'NONE',  ( 33.67500000054622689, 24.28113015263587116, 96.68563167572563088 ) ) ;
#9342 = CARTESIAN_POINT ( 'NONE',  ( 35.39999999999998437, 27.13292387221364876, 88.47553407664153724 ) ) ;
#9343 = CIRCLE ( 'NONE', #3860, 7.500000000000000000 ) ;
#9344 = CARTESIAN_POINT ( 'NONE',  ( -3.256860162955865334, 29.47720352819935030, 20.75492283549158401 ) ) ;
#9345 = CARTESIAN_POINT ( 'NONE',  ( 39.97500000054622404, 15.71886984736413417, 96.68563167572563088 ) ) ;
#9346 = EDGE_LOOP ( 'NONE', ( #10281, #1476, #1869, #1663, #10813, #6753, #4879, #6807, #1315, #3229, #11554 ) ) ;
#9347 = CARTESIAN_POINT ( 'NONE',  ( 20.95000000109246230, 26.37988106264029398, 86.15790661882942914 ) ) ;
#9348 = CARTESIAN_POINT ( 'NONE',  ( 28.25000000109246301, 12.86707612778636012, 88.47553407664152303 ) ) ;
#9349 = EDGE_LOOP ( 'NONE', ( #1497, #3728, #12156, #9819 ) ) ;
#9350 = APPLICATION_CONTEXT ( 'automotive_design' ) ;
#9351 = CARTESIAN_POINT ( 'NONE',  ( 10.00000000000000178, 19.32777951161647323, 18.46618531261938756 ) ) ;
#9352 = VERTEX_POINT ( 'NONE', #1396 ) ;
#9353 = CARTESIAN_POINT ( 'NONE',  ( 10.00000000000000355, 20.00000000000000355, -22.91287847477919826 ) ) ;
#9354 = AXIS2_PLACEMENT_3D ( 'NONE', #5353, #6239, #10231 ) ;
#9355 = CARTESIAN_POINT ( 'NONE',  ( 27.49999999999999645, 20.00000000000000355, 189.9999999999999716 ) ) ;
#9356 = FACE_OUTER_BOUND ( 'NONE', #12505, .T. ) ;
#9357 = EDGE_CURVE ( 'NONE', #8287, #1936, #3878, .T. ) ;
#9358 = DIRECTION ( 'NONE',  ( -1.000000000000000000, -0.000000000000000000, -0.000000000000000000 ) ) ;
#9359 = CARTESIAN_POINT ( 'NONE',  ( 24.87500000054622618, 22.36655054427230382, 83.50966788445364841 ) ) ;
#9360 = CARTESIAN_POINT ( 'NONE',  ( 27.97500000054622404, 17.63344945572769973, 98.07665518445361386 ) ) ;
#9361 = DIRECTION ( 'NONE',  ( 1.000000000000000000, 0.000000000000000000, 0.000000000000000000 ) ) ;
#9362 = DIRECTION ( 'NONE',  ( 1.000000000000000000, 0.000000000000000000, -0.000000000000000000 ) ) ;
#9363 = ORIENTED_EDGE ( 'NONE', *, *, #4811, .T. ) ;
#9364 = CARTESIAN_POINT ( 'NONE',  ( 39.95000000109245519, 13.62011893735971135, 95.42841645007781892 ) ) ;
#9365 = CARTESIAN_POINT ( 'NONE',  ( 10.00000000000000533, 19.33140358361892552, 22.91287847477920891 ) ) ;
#9366 = ORIENTED_EDGE ( 'NONE', *, *, #8676, .T. ) ;
#9367 = LINE ( 'NONE', #8409, #3829 ) ;
#9368 = ORIENTED_EDGE ( 'NONE', *, *, #9935, .T. ) ;
#9369 = EDGE_CURVE ( 'NONE', #8125, #2736, #7817, .T. ) ;
#9370 = CARTESIAN_POINT ( 'NONE',  ( -8.122732253212674891, 14.15824396964088372, -23.64440389997412950 ) ) ;
#9371 = CARTESIAN_POINT ( 'NONE',  ( 6.613906629224937106, 12.49257982187926785, -19.93301561218848761 ) ) ;
#9372 = DIRECTION ( 'NONE',  ( -1.000000000000000000, -0.000000000000000000, -0.000000000000000000 ) ) ;
#9373 = CYLINDRICAL_SURFACE ( 'NONE', #1106, 10.00000000000000355 ) ;
#9374 = CARTESIAN_POINT ( 'NONE',  ( 27.99999999999998579, 20.00000000000000355, 98.29316153445363113 ) ) ;
#9375 = CARTESIAN_POINT ( 'NONE',  ( -9.737903098387532097, 17.70124625263684592, 18.60587983635906539 ) ) ;
#9376 = CARTESIAN_POINT ( 'NONE',  ( 47.65000000109246514, 20.00000000000000355, 98.29316153445363113 ) ) ;
#9377 = CARTESIAN_POINT ( 'NONE',  ( 29.47500000054622404, 26.19570976099943493, 95.29460816699764791 ) ) ;
#9378 = FACE_OUTER_BOUND ( 'NONE', #4655, .T. ) ;
#9379 = CARTESIAN_POINT ( 'NONE',  ( -3.049660161009143611, 53.97562969122508747, 24.81478968795947537 ) ) ;
#9380 = ORIENTED_EDGE ( 'NONE', *, *, #7218, .T. ) ;
#9381 = DIRECTION ( 'NONE',  ( -1.000000000000000000, -0.000000000000000000, -0.000000000000000000 ) ) ;
#9382 = ADVANCED_FACE ( 'NONE', ( #1040 ), #11687, .F. ) ;
#9383 = DIRECTION ( 'NONE',  ( 0.000000000000000000, 0.5000000000000012212, 0.8660254037844379305 ) ) ;
#9384 = CARTESIAN_POINT ( 'NONE',  ( 36.07500000054622546, 13.80429023900056507, 95.29460816699764791 ) ) ;
#9385 = CARTESIAN_POINT ( 'NONE',  ( 36.87500000054622262, 20.00000000000000355, 83.50966788445364841 ) ) ;
#9386 = CARTESIAN_POINT ( 'NONE',  ( 26.97500000054622760, 24.28113015263587471, 84.90069139318163138 ) ) ;
#9387 = CARTESIAN_POINT ( 'NONE',  ( 0.6000000000000033085, 0.000000000000000000, 0.000000000000000000 ) ) ;
#9388 = CARTESIAN_POINT ( 'NONE',  ( 3.061617023331388775E-15, 45.00000000000000711, 25.00000000000000000 ) ) ;
#9389 = EDGE_CURVE ( 'NONE', #8038, #2911, #8842, .T. ) ;
#9390 = AXIS2_PLACEMENT_3D ( 'NONE', #5837, #11737, #9709 ) ;
#9391 = CYLINDRICAL_SURFACE ( 'NONE', #2109, 21.00000000000000000 ) ;
#9392 = VERTEX_POINT ( 'NONE', #7471 ) ;
#9393 = DIRECTION ( 'NONE',  ( -0.000000000000000000, -0.000000000000000000, 1.000000000000000000 ) ) ;
#9394 = CARTESIAN_POINT ( 'NONE',  ( 0.000000000000000000, 50.00000000000000000, -28.00000000000000711 ) ) ;
#9395 =( NAMED_UNIT ( * ) SI_UNIT ( $, .STERADIAN. ) SOLID_ANGLE_UNIT ( ) );
#9396 = CARTESIAN_POINT ( 'NONE',  ( 31.57500000054622191, 26.19570976099943849, 95.29460816699764791 ) ) ;
#9397 = CARTESIAN_POINT ( 'NONE',  ( 42.99999999999999289, 20.00000000000000355, 83.29316153445364534 ) ) ;
#9398 = PRODUCT_DEFINITION_FORMATION_WITH_SPECIFIED_SOURCE ( 'ANY', '', #8, .NOT_KNOWN. ) ;
#9399 = CARTESIAN_POINT ( 'NONE',  ( 48.67500000054623399, 17.63344945572770328, 83.50966788445364841 ) ) ;
#9400 = CARTESIAN_POINT ( 'NONE',  ( 35.47500000054622404, 26.92701409722686634, 93.04388485072563242 ) ) ;
#9401 = CARTESIAN_POINT ( 'NONE',  ( 29.39999999999998792, 27.13292387221364876, 88.47553407664153724 ) ) ;
#9402 = EDGE_CURVE ( 'NONE', #1221, #5152, #8673, .T. ) ;
#9403 = CARTESIAN_POINT ( 'NONE',  ( -1.654777828561690312, 29.86772917176804398, 20.93725631092291906 ) ) ;
#9404 = CARTESIAN_POINT ( 'NONE',  ( 38.07500000054623257, 13.80429023900056507, 95.29460816699764791 ) ) ;
#9405 = EDGE_LOOP ( 'NONE', ( #2627, #6885, #40, #1619 ) ) ;
#9406 = AXIS2_PLACEMENT_3D ( 'NONE', #8026, #4085, #3136 ) ;
#9407 = CARTESIAN_POINT ( 'NONE',  ( 19.75000000109246301, 17.56310227825320425, 98.29316153445363113 ) ) ;
#9408 = CARTESIAN_POINT ( 'NONE',  ( -3.051146662956820688, 46.02554824080852569, -20.77895220992095560 ) ) ;
#9409 = ORIENTED_EDGE ( 'NONE', *, *, #2844, .F. ) ;
#9410 = CONICAL_SURFACE ( 'NONE', #12241, 5.057500000000000107, 1.047197551196592302 ) ;
#9411 = CARTESIAN_POINT ( 'NONE',  ( 2.619390655685069014, 10.34347335722847916, 20.83845118924497086 ) ) ;
#9412 = ORIENTED_EDGE ( 'NONE', *, *, #10476, .T. ) ;
#9414 = EDGE_CURVE ( 'NONE', #11966, #4281, #9661, .T. ) ;
#9413 =( BOUNDED_CURVE ( )  B_SPLINE_CURVE ( 2, ( #3582, #4790, #3767, #3703, #3833, #11329, #9493, #5621, #12404, #7584, #4663 ),
 .UNSPECIFIED., .F., .F. ) 
 B_SPLINE_CURVE_WITH_KNOTS ( ( 3, 2, 2, 2, 2, 3 ),
 ( 0.5999999999999999778, 0.6066666666666666874, 0.6133333333333332860, 0.6199999999999999956, 0.6266666666666667052, 0.6333333333333333037 ),
 .UNSPECIFIED. ) 
 CURVE ( )  GEOMETRIC_REPRESENTATION_ITEM ( )  RATIONAL_B_SPLINE_CURVE ( ( 1.000000000000000000, 0.9510565162951535312, 1.000000000000000000, 0.9510565162951535312, 1.000000000000000000, 0.9510565162951535312, 1.000000000000000000, 0.9510565162951535312, 1.000000000000000000, 0.9510565162951535312, 1.000000000000000000 ) ) 
 REPRESENTATION_ITEM ( '' )  );
#9415 = CARTESIAN_POINT ( 'NONE',  ( 6.601689117734505174, 27.51820487403981375, -24.11400268645312650 ) ) ;
#9416 = LINE ( 'NONE', #12265, #3836 ) ;
#9417 = CARTESIAN_POINT ( 'NONE',  ( -3.294598684565033704E-22, 45.00000000000000711, -28.00000000000000355 ) ) ;
#9418 = CARTESIAN_POINT ( 'NONE',  ( 41.35889894354065177, 20.00000000000000355, 197.9999999999999716 ) ) ;
#9419 = CARTESIAN_POINT ( 'NONE',  ( 25.37500000054622973, 26.92701409722686634, 93.04388485072563242 ) ) ;
#9420 = CARTESIAN_POINT ( 'NONE',  ( 21.27500000054622475, 26.92701409722686634, 88.54243821818162985 ) ) ;
#9421 = VECTOR ( 'NONE', #4731, 1000.000000000000114 ) ;
#9422 = CARTESIAN_POINT ( 'NONE',  ( -2.610103423518925769, 29.65902056345734650, -24.86541183722168213 ) ) ;
#9423 = CARTESIAN_POINT ( 'NONE',  ( -50.00000000000001421, 40.00000000000000000, 121.2488769092545198 ) ) ;
#9424 = ORIENTED_EDGE ( 'NONE', *, *, #11859, .F. ) ;
#9425 = CARTESIAN_POINT ( 'NONE',  ( 35.15000000109247225, 27.88596668178699645, 90.79316153445363113 ) ) ;
#9426 = CARTESIAN_POINT ( 'NONE',  ( 24.29999999999999005, 13.62011893735970958, 95.42841645007781892 ) ) ;
#9427 = ORIENTED_EDGE ( 'NONE', *, *, #4278, .F. ) ;
#9428 = FACE_OUTER_BOUND ( 'NONE', #6343, .T. ) ;
#9429 = ORIENTED_EDGE ( 'NONE', *, *, #3853, .T. ) ;
#9430 = CARTESIAN_POINT ( 'NONE',  ( 4.337336347961448624, 52.50902530749537078, 20.54804625155474440 ) ) ;
#9431 = CARTESIAN_POINT ( 'NONE',  ( 10.00000000000000355, 20.00000000000000355, -18.46618531261938401 ) ) ;
#9432 = VECTOR ( 'NONE', #11838, 1000.000000000000000 ) ;
#9433 = DIRECTION ( 'NONE',  ( -1.000000000000000000, -0.000000000000000000, -0.000000000000000000 ) ) ;
#9434 = CARTESIAN_POINT ( 'NONE',  ( 0.000000000000000000, 20.00000000000000355, -66.99999999999998579 ) ) ;
#9435 = DIRECTION ( 'NONE',  ( 0.000000000000000000, 0.000000000000000000, -1.000000000000000000 ) ) ;
#9436 = CARTESIAN_POINT ( 'NONE',  ( -31.74999999999995737, 0.000000000000000000, 6.000000000000003553 ) ) ;
#9437 = CARTESIAN_POINT ( 'NONE',  ( 10.40000000000000036, 0.000000000000000000, 0.000000000000000000 ) ) ;
#9438 = CARTESIAN_POINT ( 'NONE',  ( 49.67500000054622689, 24.28113015263587116, 96.68563167572563088 ) ) ;
#9439 = CARTESIAN_POINT ( 'NONE',  ( 7.519126441075570710, 26.60062706338189642, 23.84344315696457173 ) ) ;
#9440 = CARTESIAN_POINT ( 'NONE',  ( 46.75000000109247367, 22.43689772174677088, 83.29316153445361692 ) ) ;
#9441 = ORIENTED_EDGE ( 'NONE', *, *, #2201, .T. ) ;
#9442 = VERTEX_POINT ( 'NONE', #1576 ) ;
#9443 = VECTOR ( 'NONE', #6697, 1000.000000000000000 ) ;
#9444 = B_SPLINE_CURVE_WITH_KNOTS ( 'NONE', 3,
 ( #808, #9569, #5762, #4742, #9631, #746, #4681, #941, #7599, #5823, #11660, #12479, #4870, #2773, #3782, #7662, #6702, #10569, #9607, #6576, #6831, #3659, #7534, #11402, #2712, #10441 ),
 .UNSPECIFIED., .F., .F.,
 ( 4, 2, 2, 2, 2, 2, 2, 2, 2, 2, 2, 2, 4 ),
 ( 3.701750345114177145E-18, 0.001985659510702812366, 0.002978489266054215080, 0.003971319021405616927, 0.005956978532108423222, 0.006949808287459825068, 0.007942638042811226914, 0.008935467798162625291, 0.009928297553514025403, 0.01191395706421683257, 0.01290678681956823615, 0.01389961657491964146, 0.01588527608562245730 ),
 .UNSPECIFIED. ) ;
#9445 = ADVANCED_BREP_SHAPE_REPRESENTATION ( '', ( #2150, #9021 ), #3536 ) ;
#9446 = CARTESIAN_POINT ( 'NONE',  ( 27.49999999999999645, 20.00000000000000355, 171.0000000000000000 ) ) ;
#9447 = CARTESIAN_POINT ( 'NONE',  ( 38.47500000054622404, 13.07298590277314432, 88.54243821818161564 ) ) ;
#9448 = CARTESIAN_POINT ( 'NONE',  ( 23.57500000054622902, 24.28113015263587116, 96.68563167572563088 ) ) ;
#9449 = EDGE_CURVE ( 'NONE', #6737, #2324, #6513, .T. ) ;
#9450 = CARTESIAN_POINT ( 'NONE',  ( 0.000000000000000000, 70.00000000000000000, 0.000000000000000000 ) ) ;
#9451 = CARTESIAN_POINT ( 'NONE',  ( 3.974960981574284347, 46.94936902441865101, 24.68265737646872893 ) ) ;
#9452 = DIRECTION ( 'NONE',  ( -1.000000000000000000, -0.000000000000000000, -0.000000000000000000 ) ) ;
#9453 = DIRECTION ( 'NONE',  ( -0.000000000000000000, -0.000000000000000000, 1.000000000000000000 ) ) ;
#9454 = ADVANCED_FACE ( 'NONE', ( #12172 ), #5388, .T. ) ;
#9455 = DIRECTION ( 'NONE',  ( -1.000000000000000000, -0.000000000000000000, -0.000000000000000000 ) ) ;
#9456 = ORIENTED_EDGE ( 'NONE', *, *, #3507, .T. ) ;
#9457 =( BOUNDED_CURVE ( )  B_SPLINE_CURVE ( 2, ( #8784, #37, #9745, #7839, #10681, #10616, #3898, #7776, #2954, #1992, #103 ),
 .UNSPECIFIED., .F., .F. ) 
 B_SPLINE_CURVE_WITH_KNOTS ( ( 3, 2, 2, 2, 2, 3 ),
 ( 0.4666666666666666186, 0.4733333333333332726, 0.4799999999999999267, 0.4866666666666666918, 0.4933333333333333459, 0.5000000000000000000 ),
 .UNSPECIFIED. ) 
 CURVE ( )  GEOMETRIC_REPRESENTATION_ITEM ( )  RATIONAL_B_SPLINE_CURVE ( ( 1.000000000000000444, 0.9510565162951531981, 1.000000000000000000, 0.9510565162951535312, 1.000000000000000000, 0.9510565162951535312, 1.000000000000000000, 0.9510565162951535312, 1.000000000000000000, 0.9510565162951535312, 1.000000000000000000 ) ) 
 REPRESENTATION_ITEM ( '' )  );
#9458 = DIRECTION ( 'NONE',  ( 0.000000000000000000, 0.000000000000000000, -1.000000000000000000 ) ) ;
#9459 = DIRECTION ( 'NONE',  ( 1.000000000000000000, 0.000000000000000000, 0.000000000000000000 ) ) ;
#9460 = CIRCLE ( 'NONE', #11898, 17.50000000000000000 ) ;
#9461 = CARTESIAN_POINT ( 'NONE',  ( 26.27500000054622475, 13.07298590277314254, 93.04388485072563242 ) ) ;
#9462 = CARTESIAN_POINT ( 'NONE',  ( 0.000000000000000000, 139.9999999999999716, -21.00000000000000000 ) ) ;
#9463 = CARTESIAN_POINT ( 'NONE',  ( 39.97500000054622404, 15.71886984736413417, 96.68563167572563088 ) ) ;
#9464 = CARTESIAN_POINT ( 'NONE',  ( 29.07500000054622191, 24.28113015263587471, 84.90069139318163138 ) ) ;
#9465 = CARTESIAN_POINT ( 'NONE',  ( 32.89999999999998437, 17.56310227825321135, 83.29316153445363113 ) ) ;
#9466 = CARTESIAN_POINT ( 'NONE',  ( 30.39999999999998792, 12.86707612778636012, 93.11078899226572503 ) ) ;
#9467 = CARTESIAN_POINT ( 'NONE',  ( 40.57500000054623257, 15.71886984736413773, 84.90069139318163138 ) ) ;
#9468 = ORIENTED_EDGE ( 'NONE', *, *, #1189, .F. ) ;
#9469 = EDGE_CURVE ( 'NONE', #10329, #11133, #12294, .T. ) ;
#9470 = CARTESIAN_POINT ( 'NONE',  ( 47.17500000054623399, 26.92701409722686634, 88.54243821818162985 ) ) ;
#9471 = CARTESIAN_POINT ( 'NONE',  ( 6.000000000000000000, 0.000000000000000000, 0.000000000000000000 ) ) ;
#9472 = EDGE_LOOP ( 'NONE', ( #2246, #4995 ) ) ;
#9473 = DIRECTION ( 'NONE',  ( 1.000000000000000000, -0.000000000000000000, -0.000000000000000000 ) ) ;
#9474 = ORIENTED_EDGE ( 'NONE', *, *, #10533, .T. ) ;
#9475 = CARTESIAN_POINT ( 'NONE',  ( 8.964356567778166252, 24.44381301785154292, -23.33811713236289620 ) ) ;
#9476 = CARTESIAN_POINT ( 'NONE',  ( 43.09999999999998721, 22.43689772174680641, 83.29316153445363113 ) ) ;
#9477 = ADVANCED_FACE ( 'NONE', ( #2583 ), #5574, .T. ) ;
#9478 = PLANE ( 'NONE',  #7031 ) ;
#9479 = CARTESIAN_POINT ( 'NONE',  ( 42.67500000054622689, 15.71886984736413773, 84.90069139318163138 ) ) ;
#9480 = DIRECTION ( 'NONE',  ( -0.000000000000000000, -0.000000000000000000, -1.000000000000000000 ) ) ;
#9481 = AXIS2_PLACEMENT_3D ( 'NONE', #1239, #4853, #6875 ) ;
#9482 = CARTESIAN_POINT ( 'NONE',  ( 47.59999999999998721, 27.13292387221364876, 93.11078899226573924 ) ) ;
#9483 = CARTESIAN_POINT ( 'NONE',  ( -3.242423582264189807, 29.46551675503955536, -24.79088612835948879 ) ) ;
#9484 = ADVANCED_FACE ( 'NONE', ( #5326 ), #10455, .F. ) ;
#9485 = DIRECTION ( 'NONE',  ( -0.000000000000000000, -0.000000000000000000, 1.000000000000000000 ) ) ;
#9486 = VERTEX_POINT ( 'NONE', #9196 ) ;
#9487 = CARTESIAN_POINT ( 'NONE',  ( 38.85000000109246798, 24.40838939219355197, 84.72553407664153724 ) ) ;
#9488 = CARTESIAN_POINT ( 'NONE',  ( 9.353363810095283171, 16.44731154698707698, 23.18475774758237407 ) ) ;
#9489 = ORIENTED_EDGE ( 'NONE', *, *, #8850, .F. ) ;
#9490 = VERTEX_POINT ( 'NONE', #8242 ) ;
#9491 = CARTESIAN_POINT ( 'NONE',  ( 27.49999999999999645, 20.00000000000000355, 162.0000000000000000 ) ) ;
#9492 = ADVANCED_FACE ( 'NONE', ( #7406 ), #3414, .F. ) ;
#9493 = CARTESIAN_POINT ( 'NONE',  ( 31.05000000109246372, 27.13292387221364876, 88.47553407664153724 ) ) ;
#9494 = CARTESIAN_POINT ( 'NONE',  ( -8.961327849752377617, 24.44988401922752530, 23.33927995079777062 ) ) ;
#9495 = AXIS2_PLACEMENT_3D ( 'NONE', #2320, #10126, #1373 ) ;
#9496 = LINE ( 'NONE', #674, #2947 ) ;
#9497 = FACE_OUTER_BOUND ( 'NONE', #6130, .T. ) ;
#9498=STYLED_ITEM('',(#12591),#2064);
#9499 = CARTESIAN_POINT ( 'NONE',  ( 42.65000000109246514, 20.00000000000000355, 83.29316153445364534 ) ) ;
#9500 = CARTESIAN_POINT ( 'NONE',  ( 48.55000000109247082, 17.56310227825320069, 83.29316153445363113 ) ) ;
#9501 = CARTESIAN_POINT ( 'NONE',  ( 48.67500000054622689, 15.71886984736413773, 84.90069139318163138 ) ) ;
#9502 = CARTESIAN_POINT ( 'NONE',  ( -27.49999999999999645, 27.49999999999999645, 145.0000000000000000 ) ) ;
#9503 = CARTESIAN_POINT ( 'NONE',  ( 27.50000000000000355, 12.50000000000001066, 145.0000000000000000 ) ) ;
#9504 = VERTEX_POINT ( 'NONE', #9261 ) ;
#9505 = VECTOR ( 'NONE', #6203, 1000.000000000000000 ) ;
#9506 = ORIENTED_EDGE ( 'NONE', *, *, #482, .T. ) ;
#9507 = CIRCLE ( 'NONE', #7270, 25.00000000000000000 ) ;
#9508 = CARTESIAN_POINT ( 'NONE',  ( -50.00000000000001421, 20.00000000000000000, 145.0000000000000000 ) ) ;
#9509 = DIRECTION ( 'NONE',  ( 0.000000000000000000, 0.000000000000000000, 1.000000000000000000 ) ) ;
#9510 = CARTESIAN_POINT ( 'NONE',  ( 39.67500000054622689, 24.28113015263587116, 96.68563167572563088 ) ) ;
#9511 = CARTESIAN_POINT ( 'NONE',  ( 21.67500000054622689, 22.36655054427230027, 98.07665518445361386 ) ) ;
#9512 = DIRECTION ( 'NONE',  ( 0.000000000000000000, 1.224646799147353207E-16, 1.000000000000000000 ) ) ;
#9513 =( REPRESENTATION_RELATIONSHIP ('NONE','NONE', #4262, #1739 ) REPRESENTATION_RELATIONSHIP_WITH_TRANSFORMATION ( #10835 )SHAPE_REPRESENTATION_RELATIONSHIP( ) );
#9514 = DIRECTION ( 'NONE',  ( -0.000000000000000000, -0.000000000000000000, 1.000000000000000000 ) ) ;
#9515 = CYLINDRICAL_SURFACE ( 'NONE', #4443, 6.000000000000000000 ) ;
#9516 = DIRECTION ( 'NONE',  ( 0.000000000000000000, 0.000000000000000000, 1.000000000000000000 ) ) ;
#9517 = VECTOR ( 'NONE', #3085, 1000.000000000000114 ) ;
#9518 = LINE ( 'NONE', #1646, #9749 ) ;
#9519 = ORIENTED_EDGE ( 'NONE', *, *, #4743, .F. ) ;
#9520 = LINE ( 'NONE', #7547, #6909 ) ;
#9521 = EDGE_CURVE ( 'NONE', #5616, #5913, #6456, .T. ) ;
#9522 = DIRECTION ( 'NONE',  ( 1.000000000000000000, 0.000000000000000000, 0.000000000000000000 ) ) ;
#9523 = CARTESIAN_POINT ( 'NONE',  ( 24.37500000054621907, 12.34168156654572357, 90.79316153445363113 ) ) ;
#9524 = CARTESIAN_POINT ( 'NONE',  ( 36.59999999999998721, 12.86707612778636012, 88.47553407664152303 ) ) ;
#9525 = CARTESIAN_POINT ( 'NONE',  ( 39.47500000054622404, 26.19570976099943849, 95.29460816699764791 ) ) ;
#9526 = CARTESIAN_POINT ( 'NONE',  ( 29.47500000054622404, 26.92701409722686634, 93.04388485072563242 ) ) ;
#9527 = CARTESIAN_POINT ( 'NONE',  ( 27.79999999999998650, 24.40838939219354842, 96.86078899226572503 ) ) ;
#9528 = FACE_OUTER_BOUND ( 'NONE', #4992, .T. ) ;
#9529 = CARTESIAN_POINT ( 'NONE',  ( 41.07500000054622546, 26.19570976099943493, 86.29171490190961435 ) ) ;
#9530 = ORIENTED_EDGE ( 'NONE', *, *, #4175, .F. ) ;
#9531 = AXIS2_PLACEMENT_3D ( 'NONE', #4833, #9, #8755 ) ;
#9532 = CARTESIAN_POINT ( 'NONE',  ( 48.47500000054623115, 13.80429023900056684, 86.29171490190961435 ) ) ;
#9533 = DIRECTION ( 'NONE',  ( 0.000000000000000000, -1.000000000000000000, 0.000000000000000000 ) ) ;
#9534 = ORIENTED_EDGE ( 'NONE', *, *, #1944, .F. ) ;
#9535 = CARTESIAN_POINT ( 'NONE',  ( 5.033147323133203344, 11.33447346640459230, 20.39563185274203150 ) ) ;
#9536 = ORIENTED_EDGE ( 'NONE', *, *, #2468, .T. ) ;
#9537 = CARTESIAN_POINT ( 'NONE',  ( 9.739799295956466096, 22.29052955100696920, -23.02479834983350671 ) ) ;
#9538 = DIRECTION ( 'NONE',  ( 0.000000000000000000, 0.000000000000000000, 1.000000000000000000 ) ) ;
#9539 = CARTESIAN_POINT ( 'NONE',  ( 2.216731485194162854, 45.50631650129702166, -27.91375863587312267 ) ) ;
#9540 = AXIS2_PLACEMENT_3D ( 'NONE', #8067, #6284, #7231 ) ;
#9541 = CARTESIAN_POINT ( 'NONE',  ( 42.17500000054622689, 13.80429023900056507, 95.29460816699764791 ) ) ;
#9542 = CARTESIAN_POINT ( 'NONE',  ( 1.000000000000000888, 20.00000000000000355, 189.9999999999999716 ) ) ;
#9543 = EDGE_CURVE ( 'NONE', #9504, #11262, #6814, .T. ) ;
#9544 = CARTESIAN_POINT ( 'NONE',  ( -1.613768212969407978, 45.25637963430527577, -27.95508518501520001 ) ) ;
#9545 = CARTESIAN_POINT ( 'NONE',  ( 47.27500000054622831, 26.92701409722686634, 88.54243821818162985 ) ) ;
#9546 = CARTESIAN_POINT ( 'NONE',  ( 21.77500000054622831, 22.36655054427230027, 98.07665518445361386 ) ) ;
#9547 = DIRECTION ( 'NONE',  ( 0.000000000000000000, 0.000000000000000000, -1.000000000000000000 ) ) ;
#9548 = CARTESIAN_POINT ( 'NONE',  ( 39.15000000109246514, 27.88596668178699645, 90.79316153445363113 ) ) ;
#9549 = VERTEX_POINT ( 'NONE', #5514 ) ;
#9550 = CARTESIAN_POINT ( 'NONE',  ( 38.95000000109246940, 26.37988106264029398, 86.15790661882942914 ) ) ;
#9551 = CARTESIAN_POINT ( 'NONE',  ( 10.00000000000000355, 20.00000000000000355, 22.91287847477919826 ) ) ;
#9552 = ORIENTED_EDGE ( 'NONE', *, *, #10663, .T. ) ;
#9553 = VERTEX_POINT ( 'NONE', #684 ) ;
#9554 = CARTESIAN_POINT ( 'NONE',  ( 19.82500000054622546, 20.00000000000000355, 98.07665518445361386 ) ) ;
#9555 = CARTESIAN_POINT ( 'NONE',  ( 7.538096365933896870, 13.39748730115788966, -19.60640367412442231 ) ) ;
#9556 = LINE ( 'NONE', #6622, #7572 ) ;
#9557 = CARTESIAN_POINT ( 'NONE',  ( -36.00000000000001421, 77.00000000000000000, 104.8533255156881836 ) ) ;
#9558 = CARTESIAN_POINT ( 'NONE',  ( -4.743623831329197849, 48.38606213893405794, 20.45762700453146721 ) ) ;
#9559 = VERTEX_POINT ( 'NONE', #12358 ) ;
#9560 = CARTESIAN_POINT ( 'NONE',  ( 27.49999999999999645, 20.00000000000000355, 170.9999999999999716 ) ) ;
#9561 = ADVANCED_FACE ( 'NONE', ( #10630 ), #12418, .F. ) ;
#9562 = CARTESIAN_POINT ( 'NONE',  ( -1.322843585767942365, 10.08231100245556000, 27.97069189717537796 ) ) ;
#9563 = CARTESIAN_POINT ( 'NONE',  ( 22.37500000054622973, 13.07298590277314432, 88.54243821818161564 ) ) ;
#9564 = CARTESIAN_POINT ( 'NONE',  ( 46.15000000109246514, 12.11403331821300533, 90.79316153445363113 ) ) ;
#9565 = CARTESIAN_POINT ( 'NONE',  ( 4.743041305584357659, 51.61559430690765282, -20.45776197285908538 ) ) ;
#9566 = ORIENTED_EDGE ( 'NONE', *, *, #10366, .T. ) ;
#9567 = ORIENTED_EDGE ( 'NONE', *, *, #3769, .F. ) ;
#9568 = EDGE_CURVE ( 'NONE', #5882, #12216, #12406, .T. ) ;
#9569 = CARTESIAN_POINT ( 'NONE',  ( -0.6720848162426399375, 30.00000000000001776, -21.00000000000000711 ) ) ;
#9570 = FACE_OUTER_BOUND ( 'NONE', #9911, .T. ) ;
#9571 = CARTESIAN_POINT ( 'NONE',  ( 10.00000000000001421, 20.25634836214397794, 98.29316153445363113 ) ) ;
#9572 = DIRECTION ( 'NONE',  ( -1.000000000000000000, -0.000000000000000000, -0.000000000000000000 ) ) ;
#9573 = FACE_OUTER_BOUND ( 'NONE', #1598, .T. ) ;
#9574 = CARTESIAN_POINT ( 'NONE',  ( -111.8465843842649292, 84.49999999999998579, 146.8533255156881978 ) ) ;
#9575 = CARTESIAN_POINT ( 'NONE',  ( 3.971194329084580588, 46.94417401791325517, 27.71757479093061249 ) ) ;
#9576 = CARTESIAN_POINT ( 'NONE',  ( 0.000000000000000000, 5.839897972853064445, -8.673617379884035472E-15 ) ) ;
#9577 = ORIENTED_EDGE ( 'NONE', *, *, #2018, .T. ) ;
#9578 = DIRECTION ( 'NONE',  ( -1.000000000000000000, -0.000000000000000000, -0.000000000000000000 ) ) ;
#9579 = CARTESIAN_POINT ( 'NONE',  ( 0.000000000000000000, 0.000000000000000000, 0.000000000000000000 ) ) ;
#9580 = CARTESIAN_POINT ( 'NONE',  ( 26.97500000054622049, 22.36655054427230382, 83.50966788445364841 ) ) ;
#9581 = CARTESIAN_POINT ( 'NONE',  ( 49.65000000109246514, 20.00000000000000355, 98.29316153445363113 ) ) ;
#9582 = TOROIDAL_SURFACE ( 'NONE', #10785, 5.400000000000001243, 0.4000000000000000222 ) ;
#9583 = CARTESIAN_POINT ( 'NONE',  ( 38.87500000054622973, 22.36655054427230382, 83.50966788445364841 ) ) ;
#9584 = CARTESIAN_POINT ( 'NONE',  ( 24.87500000054622262, 20.00000000000000355, 83.50966788445364841 ) ) ;
#9585 = CARTESIAN_POINT ( 'NONE',  ( 31.89999999999998437, 22.43689772174679575, 98.29316153445363113 ) ) ;
#9586 = EDGE_CURVE ( 'NONE', #7533, #6436, #3849, .T. ) ;
#9587 = CARTESIAN_POINT ( 'NONE',  ( 34.87500000054623683, 22.36655054427230382, 83.50966788445364841 ) ) ;
#9588 = ORIENTED_EDGE ( 'NONE', *, *, #3384, .F. ) ;
#9589 = CARTESIAN_POINT ( 'NONE',  ( 43.97500000054623115, 15.71886984736413417, 96.68563167572563088 ) ) ;
#9590 = CARTESIAN_POINT ( 'NONE',  ( 27.65000000109246514, 20.00000000000000355, 98.29316153445363113 ) ) ;
#9591 = ORIENTED_EDGE ( 'NONE', *, *, #6919, .T. ) ;
#9592 = CARTESIAN_POINT ( 'NONE',  ( -8.965892573770299023, 24.44066166037483612, -26.52619932659681012 ) ) ;
#9593 = ORIENTED_EDGE ( 'NONE', *, *, #3281, .T. ) ;
#9594 = AXIS2_PLACEMENT_3D ( 'NONE', #5384, #5509, #1572 ) ;
#9595 = CARTESIAN_POINT ( 'NONE',  ( -3.709758735690515970E-18, 30.00000000000001066, -25.00000000000000000 ) ) ;
#9596 = CARTESIAN_POINT ( 'NONE',  ( 32.99999999999998579, 20.00000000000000355, 83.29316153445364534 ) ) ;
#9597 = CARTESIAN_POINT ( 'NONE',  ( 3.974870633954390886, 46.94939079583478048, -27.71703188956191255 ) ) ;
#9598 = CARTESIAN_POINT ( 'NONE',  ( 46.57500000054622546, 13.80429023900056684, 86.29171490190961435 ) ) ;
#9599 = CYLINDRICAL_SURFACE ( 'NONE', #12433, 7.499999999999978684 ) ;
#9600 = DIRECTION ( 'NONE',  ( 0.000000000000000000, 0.000000000000000000, -1.000000000000000000 ) ) ;
#9601 = CARTESIAN_POINT ( 'NONE',  ( 47.99999999999998579, 20.00000000000000355, 98.29316153445363113 ) ) ;
#9602 = AXIS2_PLACEMENT_3D ( 'NONE', #11826, #10876, #287 ) ;
#9603 = CYLINDRICAL_SURFACE ( 'NONE', #1308, 7.499999999999992895 ) ;
#9604 = CARTESIAN_POINT ( 'NONE',  ( -27.49999999999999645, 12.50000000000001066, 145.0000000000000000 ) ) ;
#9605 = EDGE_LOOP ( 'NONE', ( #126, #6235, #3870, #10782, #4255, #5631, #4195, #4893, #1105, #11303, #4333, #5542, #1443, #3126, #7512, #8065 ) ) ;
#9606 = CIRCLE ( 'NONE', #10408, 7.500000000000000000 ) ;
#9607 = CARTESIAN_POINT ( 'NONE',  ( -8.975987864778222303, 24.45580491392657052, -18.98708776393284836 ) ) ;
#9608 = CARTESIAN_POINT ( 'NONE',  ( 38.75000000109245946, 22.43689772174679575, 83.29316153445363113 ) ) ;
#9609 = CARTESIAN_POINT ( 'NONE',  ( 9.739739614376460963, 17.70973893131317922, 23.02482158226496622 ) ) ;
#9610 = EDGE_LOOP ( 'NONE', ( #2027, #7230, #2267, #11775 ) ) ;
#9611 = EDGE_CURVE ( 'NONE', #10746, #11119, #6610, .T. ) ;
#9612 = EDGE_LOOP ( 'NONE', ( #8838, #4091, #5371 ) ) ;
#9613 = CARTESIAN_POINT ( 'NONE',  ( 32.00000000000000000, 5.035999999999999588, 0.000000000000000000 ) ) ;
#9614 = DIRECTION ( 'NONE',  ( -1.000000000000000000, -0.000000000000000000, -0.000000000000000000 ) ) ;
#9615 = AXIS2_PLACEMENT_3D ( 'NONE', #1571, #4362, #7147 ) ;
#9616 = PRODUCT_DEFINITION ( 'UNKNOWN', '', #12436, #7007 ) ;
#9617 = CARTESIAN_POINT ( 'NONE',  ( -4.448741964560915640, 28.96190946584970405, 24.60274125495980613 ) ) ;
#9618 = EDGE_CURVE ( 'NONE', #1942, #10754, #2437, .T. ) ;
#9619 = CARTESIAN_POINT ( 'NONE',  ( 36.67500000054623399, 17.63344945572770328, 83.50966788445364841 ) ) ;
#9620 = PLANE ( 'NONE',  #112 ) ;
#9621 = CARTESIAN_POINT ( 'NONE',  ( -3.974643129415062148, 46.94910658706874784, 20.62125717344303411 ) ) ;
#9622 = VERTEX_POINT ( 'NONE', #8610 ) ;
#9623 = FACE_OUTER_BOUND ( 'NONE', #9346, .T. ) ;
#9624 = CARTESIAN_POINT ( 'NONE',  ( -0.3293999078206490405, 9.999999999999992895, 28.00000000000000000 ) ) ;
#9625 = CARTESIAN_POINT ( 'NONE',  ( 22.57500000054622902, 15.71886984736413773, 84.90069139318163138 ) ) ;
#9626 = VERTEX_POINT ( 'NONE', #871 ) ;
#9627 = CARTESIAN_POINT ( 'NONE',  ( -27.49999999999999645, 27.49999999999999645, 145.0000000000000000 ) ) ;
#9628 = CARTESIAN_POINT ( 'NONE',  ( 12.00000000000000355, 1.102182119232617714E-15, -9.000000000000000000 ) ) ;
#9629 = ORIENTED_EDGE ( 'NONE', *, *, #7190, .T. ) ;
#9630 = EDGE_LOOP ( 'NONE', ( #8165, #11309 ) ) ;
#9631 = CARTESIAN_POINT ( 'NONE',  ( -2.621352440196214495, 29.65601317703552198, -20.83821235188215226 ) ) ;
#9632 = EDGE_CURVE ( 'NONE', #11970, #1856, #9444, .T. ) ;
#9633 = CIRCLE ( 'NONE', #12268, 4.057500000000000107 ) ;
#9634 = CARTESIAN_POINT ( 'NONE',  ( 13.64110105645934290, 20.00000000000000355, 172.0000000000000000 ) ) ;
#9635 = DIRECTION ( 'NONE',  ( -1.000000000000000000, -0.000000000000000000, -0.000000000000000000 ) ) ;
#9636 = CARTESIAN_POINT ( 'NONE',  ( 48.99999999999998579, 20.00000000000000355, 83.29316153445364534 ) ) ;
#9637 = CARTESIAN_POINT ( 'NONE',  ( -28.50000000000001066, 84.49999999999998579, 146.8533255156881978 ) ) ;
#9638 = ADVANCED_FACE ( 'NONE', ( #1067 ), #3027, .F. ) ;
#9639 = CARTESIAN_POINT ( 'NONE',  ( 9.478213219505041920, 23.25438371585110886, -18.74145979309692578 ) ) ;
#9640 = CIRCLE ( 'NONE', #11062, 5.057500000000000107 ) ;
#9641 = CARTESIAN_POINT ( 'NONE',  ( 1.314997555680467389, 10.06486170053814533, 24.97384176433527969 ) ) ;
#9642 = VERTEX_POINT ( 'NONE', #9059 ) ;
#9643 = CARTESIAN_POINT ( 'NONE',  ( 7.532348232781783892, 26.60942912475959332, -23.84307605514715434 ) ) ;
#9644 = CONICAL_SURFACE ( 'NONE', #10850, 5.035999999999999588, 0.7853981633974685961 ) ;
#9645 = ADVANCED_FACE ( 'NONE', ( #370 ), #4390, .T. ) ;
#9646 = APPLICATION_PROTOCOL_DEFINITION ( 'draft international standard', 'automotive_design', 1998, #8453 ) ;
#9647 = CARTESIAN_POINT ( 'NONE',  ( 25.67500000054622333, 24.28113015263587116, 96.68563167572563088 ) ) ;
#9648 = CARTESIAN_POINT ( 'NONE',  ( 47.77500000054622120, 22.36655054427230027, 98.07665518445361386 ) ) ;
#9649 = AXIS2_PLACEMENT_3D ( 'NONE', #3815, #2802, #6793 ) ;
#9650 = CARTESIAN_POINT ( 'NONE',  ( 38.47500000054621694, 13.80429023900056684, 86.29171490190961435 ) ) ;
#9651 = CARTESIAN_POINT ( 'NONE',  ( 27.07500000054622546, 24.28113015263587471, 84.90069139318163138 ) ) ;
#9652 = CARTESIAN_POINT ( 'NONE',  ( 28.49999999999998934, 12.11403331821300533, 90.79316153445363113 ) ) ;
#9653 = AXIS2_PLACEMENT_3D ( 'NONE', #1561, #6319, #9178 ) ;
#9654 = CARTESIAN_POINT ( 'NONE',  ( 34.59999999999999432, 12.86707612778636012, 88.47553407664152303 ) ) ;
#9655 = CARTESIAN_POINT ( 'NONE',  ( 35.37500000054622973, 26.92701409722686634, 93.04388485072563242 ) ) ;
#9656 = ORIENTED_EDGE ( 'NONE', *, *, #7518, .T. ) ;
#9657 = DIRECTION ( 'NONE',  ( 0.000000000000000000, 0.000000000000000000, -1.000000000000000000 ) ) ;
#9658 = ORIENTED_EDGE ( 'NONE', *, *, #2235, .F. ) ;
#9659 = DIRECTION ( 'NONE',  ( -0.5000000000000046629, 0.000000000000000000, 0.8660254037844359321 ) ) ;
#9660 = EDGE_LOOP ( 'NONE', ( #9591, #4836 ) ) ;
#9661 = CIRCLE ( 'NONE', #2771, 7.500000000000000000 ) ;
#9662 = CARTESIAN_POINT ( 'NONE',  ( 12.59999999999999964, 7.347880794884119736E-16, -6.000000000000000000 ) ) ;
#9663 = DIRECTION ( 'NONE',  ( 0.000000000000000000, 0.000000000000000000, -1.000000000000000000 ) ) ;
#9664 = CARTESIAN_POINT ( 'NONE',  ( 44.07500000054622546, 15.71886984736413417, 96.68563167572563088 ) ) ;
#9665 = CARTESIAN_POINT ( 'NONE',  ( -50.00000000000001421, 0.000000000000000000, 69.99999999999998579 ) ) ;
#9666 = CARTESIAN_POINT ( 'NONE',  ( 44.37500000054622262, 12.34168156654572535, 90.79316153445363113 ) ) ;
#9667 = CARTESIAN_POINT ( 'NONE',  ( 48.59999999999998721, 12.86707612778636012, 88.47553407664152303 ) ) ;
#9668 = VECTOR ( 'NONE', #10695, 1000.000000000000000 ) ;
#9669 = DIRECTION ( 'NONE',  ( -0.000000000000000000, -1.000000000000000000, -0.000000000000000000 ) ) ;
#9670 = DIRECTION ( 'NONE',  ( 0.000000000000000000, 0.8660254037844379305, -0.5000000000000014433 ) ) ;
#9671 = ORIENTED_EDGE ( 'NONE', *, *, #7728, .F. ) ;
#9672 = CARTESIAN_POINT ( 'NONE',  ( 29.75000000109245946, 17.56310227825320425, 98.29316153445363113 ) ) ;
#9673 = CARTESIAN_POINT ( 'NONE',  ( 2.502435999373153308, 45.66817884423451801, -24.87486459250430926 ) ) ;
#9674 = ORIENTED_EDGE ( 'NONE', *, *, #3042, .F. ) ;
#9675 = ORIENTED_EDGE ( 'NONE', *, *, #2948, .F. ) ;
#9676 = DIRECTION ( 'NONE',  ( -1.000000000000000000, -0.000000000000000000, -0.000000000000000000 ) ) ;
#9677 = VECTOR ( 'NONE', #7959, 1000.000000000000000 ) ;
#9678 = CARTESIAN_POINT ( 'NONE',  ( 0.000000000000000000, 0.000000000000000000, 0.000000000000000000 ) ) ;
#9679 = EDGE_CURVE ( 'NONE', #11614, #5090, #6137, .T. ) ;
#9680 = LINE ( 'NONE', #988, #5561 ) ;
#9681 = CARTESIAN_POINT ( 'NONE',  ( 39.27500000054622120, 27.65831843345427998, 90.79316153445363113 ) ) ;
#9682 = CARTESIAN_POINT ( 'NONE',  ( -0.6587806068097139534, 54.96719481440166533, 27.99408942736936012 ) ) ;
#9683 = CARTESIAN_POINT ( 'NONE',  ( 7.533473311303588993, 26.60795856157748673, -26.97164952521862702 ) ) ;
#9684 = FACE_OUTER_BOUND ( 'NONE', #11652, .T. ) ;
#9685 = VERTEX_POINT ( 'NONE', #10756 ) ;
#9686 = DIRECTION ( 'NONE',  ( 0.000000000000000000, 1.000000000000000000, 0.000000000000000000 ) ) ;
#9687 = DIRECTION ( 'NONE',  ( 0.000000000000000000, 0.000000000000000000, 1.000000000000000000 ) ) ;
#9688 = CARTESIAN_POINT ( 'NONE',  ( 47.87500000054622262, 20.00000000000000355, 98.07665518445361386 ) ) ;
#9689 = ORIENTED_EDGE ( 'NONE', *, *, #6277, .T. ) ;
#9690 = CARTESIAN_POINT ( 'NONE',  ( 46.45000000109246230, 15.59161060780646046, 84.72553407664153724 ) ) ;
#9691 = CARTESIAN_POINT ( 'NONE',  ( -5.000000000000000888, -3.000000000000002665, 121.2488769092545198 ) ) ;
#9692 = ORIENTED_EDGE ( 'NONE', *, *, #12244, .T. ) ;
#9693 = LINE ( 'NONE', #1006, #593 ) ;
#9694 = AXIS2_PLACEMENT_3D ( 'NONE', #2597, #4625, #10331 ) ;
#9695 = CARTESIAN_POINT ( 'NONE',  ( 21.99999999999998934, 20.00000000000000355, 98.29316153445363113 ) ) ;
#9696 = EDGE_CURVE ( 'NONE', #7152, #5818, #4931, .T. ) ;
#9697 = CARTESIAN_POINT ( 'NONE',  ( 21.47500000054622760, 26.19570976099943849, 95.29460816699764791 ) ) ;
#9698 = CARTESIAN_POINT ( 'NONE',  ( 3.764997658848628692, 46.69378447153945189, -24.71596740620162436 ) ) ;
#9699 = CARTESIAN_POINT ( 'NONE',  ( 0.000000000000000000, 31.99999999999960565, 124.8533255156881694 ) ) ;
#9700 = LINE ( 'NONE', #5769, #7157 ) ;
#9701 = CARTESIAN_POINT ( 'NONE',  ( 8.122033900404826312, 25.84264039288823511, -19.36674556122184399 ) ) ;
#9702 = AXIS2_PLACEMENT_3D ( 'NONE', #5443, #617, #7146 ) ;
#9703 = CARTESIAN_POINT ( 'NONE',  ( 7.514434402675104430, 13.39403693888593772, 23.84492327520115396 ) ) ;
#9704 = EDGE_LOOP ( 'NONE', ( #915, #2291, #9988, #3619 ) ) ;
#9705 = CARTESIAN_POINT ( 'NONE',  ( 9.466290622766221574, 23.23991477998078636, -23.13871526284164304 ) ) ;
#9706 = VECTOR ( 'NONE', #11647, 1000.000000000000000 ) ;
#9707 = EDGE_CURVE ( 'NONE', #707, #9442, #11719, .T. ) ;
#9708 = CARTESIAN_POINT ( 'NONE',  ( 20.87500000054622262, 20.00000000000000355, 83.50966788445364841 ) ) ;
#9709 = DIRECTION ( 'NONE',  ( 0.000000000000000000, 0.000000000000000000, 1.000000000000000000 ) ) ;
#9710 = CARTESIAN_POINT ( 'NONE',  ( 40.07500000054623257, 13.80429023900056507, 95.29460816699764791 ) ) ;
#9711 = AXIS2_PLACEMENT_3D ( 'NONE', #9613, #6746, #7582 ) ;
#9712 = CARTESIAN_POINT ( 'NONE',  ( 27.87500000054622262, 20.00000000000000355, 98.07665518445361386 ) ) ;
#9713 = CARTESIAN_POINT ( 'NONE',  ( 22.69999999999998153, 13.62011893735971135, 86.15790661882942914 ) ) ;
#9714 = DIRECTION ( 'NONE',  ( 1.000000000000000000, 0.000000000000000000, 0.000000000000000000 ) ) ;
#9715 = CARTESIAN_POINT ( 'NONE',  ( 33.77500000054622831, 20.00000000000000355, 98.07665518445361386 ) ) ;
#9716 = ORIENTED_EDGE ( 'NONE', *, *, #145, .T. ) ;
#9717 = EDGE_CURVE ( 'NONE', #667, #4807, #2165, .T. ) ;
#9718 = PLANE ( 'NONE',  #2017 ) ;
#9719 = VERTEX_POINT ( 'NONE', #8042 ) ;
#9720 = DIRECTION ( 'NONE',  ( 0.000000000000000000, -1.000000000000000000, 1.039664082171044481E-15 ) ) ;
#9721 = ORIENTED_EDGE ( 'NONE', *, *, #9835, .F. ) ;
#9722 = CARTESIAN_POINT ( 'NONE',  ( 43.59999999999998721, 27.13292387221364876, 93.11078899226573924 ) ) ;
#9723 = DIRECTION ( 'NONE',  ( -0.000000000000000000, -1.000000000000000000, -0.000000000000000000 ) ) ;
#9724 = EDGE_CURVE ( 'NONE', #2928, #5181, #178, .T. ) ;
#9725 = CARTESIAN_POINT ( 'NONE',  ( 46.67500000054622689, 15.71886984736413773, 84.90069139318163138 ) ) ;
#9726 = CARTESIAN_POINT ( 'NONE',  ( 27.49999999999999645, 20.00000000000000355, 188.9999999999999716 ) ) ;
#9727 = PRESENTATION_STYLE_ASSIGNMENT (( #2807 ) ) ;
#9728 = CARTESIAN_POINT ( 'NONE',  ( 43.87500000054622973, 20.00000000000000355, 98.07665518445361386 ) ) ;
#9729 = CARTESIAN_POINT ( 'NONE',  ( 43.49999999999998579, 27.88596668178699645, 90.79316153445363113 ) ) ;
#9730 = AXIS2_PLACEMENT_3D ( 'NONE', #7434, #2797, #11239 ) ;
#9731 = CARTESIAN_POINT ( 'NONE',  ( 45.49999999999997868, 27.88596668178699645, 90.79316153445363113 ) ) ;
#9732 = CARTESIAN_POINT ( 'NONE',  ( 4.999999999999997335, 40.00000000000000000, 69.99999999999998579 ) ) ;
#9733 = ORIENTED_EDGE ( 'NONE', *, *, #525, .F. ) ;
#9734 = CARTESIAN_POINT ( 'NONE',  ( 32.55000000109247082, 17.56310227825321135, 83.29316153445363113 ) ) ;
#9735 = CARTESIAN_POINT ( 'NONE',  ( -0.6638428588095105498, 10.01651532611708895, 24.99338002059894137 ) ) ;
#9736 = VERTEX_POINT ( 'NONE', #8862 ) ;
#9737 = ORIENTED_EDGE ( 'NONE', *, *, #2977, .T. ) ;
#9738 = VECTOR ( 'NONE', #2988, 1000.000000000000000 ) ;
#9739 = LINE ( 'NONE', #4662, #2616 ) ;
#9740 = CARTESIAN_POINT ( 'NONE',  ( 1.000000000000000888, 20.00000000000000711, 170.9999999999999716 ) ) ;
#9741 = LINE ( 'NONE', #2119, #3925 ) ;
#9742 =( BOUNDED_CURVE ( )  B_SPLINE_CURVE ( 2, ( #9374, #4542, #12469, #12287, #7589, #1625, #1807, #8661, #5750, #4796, #3587 ),
 .UNSPECIFIED., .F., .F. ) 
 B_SPLINE_CURVE_WITH_KNOTS ( ( 3, 2, 2, 2, 2, 3 ),
 ( 0.7333333333333332815, 0.7399999999999999911, 0.7466666666666667007, 0.7533333333333331883, 0.7599999999999998979, 0.7666666666666666075 ),
 .UNSPECIFIED. ) 
 CURVE ( )  GEOMETRIC_REPRESENTATION_ITEM ( )  RATIONAL_B_SPLINE_CURVE ( ( 1.000000000000000000, 0.9510565162951535312, 1.000000000000000000, 0.9510565162951535312, 1.000000000000000000, 0.9510565162951535312, 1.000000000000000000, 0.9510565162951535312, 1.000000000000000000, 0.9510565162951543083, 0.9999999999999992228 ) ) 
 REPRESENTATION_ITEM ( '' )  );
#9743 = CARTESIAN_POINT ( 'NONE',  ( 40.07500000054623257, 13.80429023900056507, 95.29460816699764791 ) ) ;
#9744 = CARTESIAN_POINT ( 'NONE',  ( 37.27500000054622831, 26.92701409722686634, 88.54243821818162985 ) ) ;
#9745 = CARTESIAN_POINT ( 'NONE',  ( 35.45000000109246940, 24.40838939219354842, 96.86078899226572503 ) ) ;
#9746 = CARTESIAN_POINT ( 'NONE',  ( 27.49999999999999645, 20.00000000000000355, 162.0000000000000000 ) ) ;
#9747 = CARTESIAN_POINT ( 'NONE',  ( 35.00000000000000000, 24.39339828220178674, 137.5000000000000000 ) ) ;
#9748 = ORIENTED_EDGE ( 'NONE', *, *, #4314, .T. ) ;
#9749 = VECTOR ( 'NONE', #2781, 1000.000000000000000 ) ;
#9750 = CARTESIAN_POINT ( 'NONE',  ( 47.85000000109246088, 15.59161060780645691, 96.86078899226572503 ) ) ;
#9751 = VERTEX_POINT ( 'NONE', #6953 ) ;
#9752 = EDGE_CURVE ( 'NONE', #9941, #8038, #549, .T. ) ;
#9753 = CARTESIAN_POINT ( 'NONE',  ( -27.49999999999999645, 20.00000000000000355, 170.0000119999999697 ) ) ;
#9754 = UNCERTAINTY_MEASURE_WITH_UNIT (LENGTH_MEASURE( 1.000000000000000082E-05 ), #11010, 'distance_accuracy_value', 'NONE');
#9755 = ORIENTED_EDGE ( 'NONE', *, *, #720, .F. ) ;
#9756 = ORIENTED_EDGE ( 'NONE', *, *, #11327, .F. ) ;
#9757 = AXIS2_PLACEMENT_3D ( 'NONE', #7941, #1222, #8956 ) ;
#9758 = DIRECTION ( 'NONE',  ( 0.000000000000000000, 0.000000000000000000, 1.000000000000000000 ) ) ;
#9759 = CARTESIAN_POINT ( 'NONE',  ( 1.614235646224727372, 54.74352724365349587, 24.94966740611544509 ) ) ;
#9760 = CARTESIAN_POINT ( 'NONE',  ( 6.688242141207060953, 27.43430974961319535, 89.77032832267597939 ) ) ;
#9761 = CARTESIAN_POINT ( 'NONE',  ( 37.69999999999998153, 26.37988106264029398, 95.42841645007781892 ) ) ;
#9762 = CARTESIAN_POINT ( 'NONE',  ( 5.038105599187825412, 28.64433225779773551, 20.38884022818624331 ) ) ;
#9763 = CARTESIAN_POINT ( 'NONE',  ( 4.336879845426758529, 47.49058353134505950, -20.54812575080782011 ) ) ;
#9764 = CARTESIAN_POINT ( 'NONE',  ( -28.50000000000001066, 69.50000000000000000, 146.8533255156881978 ) ) ;
#9765 = CARTESIAN_POINT ( 'NONE',  ( -111.8465843842649292, 69.50000000000000000, 146.8533255156881978 ) ) ;
#9766 = ORIENTED_EDGE ( 'NONE', *, *, #11531, .T. ) ;
#9767 = CARTESIAN_POINT ( 'NONE',  ( 7.192769615190809278E-19, 10.00000000000000000, -28.00000000000000355 ) ) ;
#9768 = EDGE_CURVE ( 'NONE', #11818, #1877, #1362, .T. ) ;
#9769 = PRODUCT_CONTEXT ( 'NONE', #1721, 'mechanical' ) ;
#9770 = CARTESIAN_POINT ( 'NONE',  ( 22.97500000054622049, 22.36655054427230382, 83.50966788445364841 ) ) ;
#9771 = CARTESIAN_POINT ( 'NONE',  ( 48.57500000054622546, 13.80429023900056684, 86.29171490190961435 ) ) ;
#9772 = ADVANCED_FACE ( 'NONE', ( #9885 ), #2154, .T. ) ;
#9773 = CARTESIAN_POINT ( 'NONE',  ( 32.37500000054622973, 13.07298590277314432, 88.54243821818161564 ) ) ;
#9774 = CARTESIAN_POINT ( 'NONE',  ( 1.317448503741515342, 10.08163033484836113, -24.96744191981147409 ) ) ;
#9775 = CARTESIAN_POINT ( 'NONE',  ( 21.59999999999998721, 27.13292387221364876, 93.11078899226573924 ) ) ;
#9776 = DIRECTION ( 'NONE',  ( 0.000000000000000000, 0.000000000000000000, -1.000000000000000000 ) ) ;
#9777 = CARTESIAN_POINT ( 'NONE',  ( 33.87500000054621552, 17.63344945572769973, 98.07665518445361386 ) ) ;
#9778 = EDGE_LOOP ( 'NONE', ( #3984, #12026, #9380, #3623 ) ) ;
#9779 = DIRECTION ( 'NONE',  ( -1.000000000000000000, 0.000000000000000000, 0.000000000000000000 ) ) ;
#9780 = ORIENTED_EDGE ( 'NONE', *, *, #4697, .F. ) ;
#9781 = CARTESIAN_POINT ( 'NONE',  ( 4.338316237973660172, 52.50713254139536446, 27.66247836308076558 ) ) ;
#9782 = EDGE_LOOP ( 'NONE', ( #4765, #6378, #2237, #9409 ) ) ;
#9783 = SHAPE_REPRESENTATION_RELATIONSHIP ( 'NONE' , 'NONE' ,  #8235, #9445 ) ;
#9784 = CARTESIAN_POINT ( 'NONE',  ( -21.00000000000001066, 77.00000000000000000, 104.8533255156881836 ) ) ;
#9785 = CARTESIAN_POINT ( 'NONE',  ( 0.000000000000000000, 5.839897972853064445, -8.673617379884035472E-15 ) ) ;
#9786 = CARTESIAN_POINT ( 'NONE',  ( 36.77500000054622831, 17.63344945572770328, 83.50966788445364841 ) ) ;
#9787 = DIRECTION ( 'NONE',  ( -1.000000000000000000, 0.000000000000000000, 0.000000000000000000 ) ) ;
#9788 = EDGE_CURVE ( 'NONE', #7590, #188, #305, .T. ) ;
#9789 = CARTESIAN_POINT ( 'NONE',  ( -0.3267093297687971853, 45.00000000000001421, -28.00000000000001421 ) ) ;
#9790 = CARTESIAN_POINT ( 'NONE',  ( 37.27500000054622831, 26.92701409722686634, 88.54243821818162985 ) ) ;
#9791 = CARTESIAN_POINT ( 'NONE',  ( 39.59999999999998721, 27.13292387221364876, 93.11078899226573924 ) ) ;
#9792 = CARTESIAN_POINT ( 'NONE',  ( -5.000000000000000888, -3.000000000000002665, 121.2488769092545198 ) ) ;
#9793 = CARTESIAN_POINT ( 'NONE',  ( 6.000000000000000000, 2.919948986426526005, -5.057500000000003659 ) ) ;
#9794 = ORIENTED_EDGE ( 'NONE', *, *, #10084, .F. ) ;
#9795 = B_SPLINE_CURVE_WITH_KNOTS ( 'NONE', 3,
 ( #11490, #9351, #772, #1779, #2677, #6663, #12446, #5727, #12506, #2799, #10345, #1843, #4641, #3809, #6540, #7563, #7689, #9535, #8393, #653, #12262, #9411, #3562, #8512, #7437, #1722 ),
 .UNSPECIFIED., .F., .F.,
 ( 4, 2, 2, 2, 2, 2, 2, 2, 2, 2, 2, 2, 4 ),
 ( 0.000000000000000000, 0.001985162064921483505, 0.002977743097382220486, 0.003970324129842958336, 0.005955486194764421023, 0.006948067227225150633, 0.007940648259685878507, 0.008933229292146606382, 0.009925810324607334256, 0.01191097238952878480, 0.01290355342198951268, 0.01389613445445023708, 0.01588129651937168763 ),
 .UNSPECIFIED. ) ;
#9796 = VECTOR ( 'NONE', #10899, 1000.000000000000000 ) ;
#9797 = CARTESIAN_POINT ( 'NONE',  ( 28.25000000109246301, 12.86707612778636012, 88.47553407664152303 ) ) ;
#9798 = CARTESIAN_POINT ( 'NONE',  ( 4.450527323037263727, 11.02130320606087821, 24.60818795580814822 ) ) ;
#9799 = VERTEX_POINT ( 'NONE', #2207 ) ;
#9800 = EDGE_CURVE ( 'NONE', #5412, #6224, #7142, .T. ) ;
#9801 = ORIENTED_EDGE ( 'NONE', *, *, #12257, .T. ) ;
#9802 = CARTESIAN_POINT ( 'NONE',  ( 3.429011039554510417E-15, 10.00000000000000000, 28.00000000000000355 ) ) ;
#9803 = CARTESIAN_POINT ( 'NONE',  ( -3.307156092220256749, 53.76411647547837447, -24.78137765757908895 ) ) ;
#9804 = CARTESIAN_POINT ( 'NONE',  ( 12.59999999999999964, 0.000000000000000000, 6.000000000000000000 ) ) ;
#9805 = CONICAL_SURFACE ( 'NONE', #1094, 25.50000000000000711, 0.7853981633974552734 ) ;
#9806 = CARTESIAN_POINT ( 'NONE',  ( 35.67500000054623399, 22.36655054427230027, 98.07665518445361386 ) ) ;
#9807 = CARTESIAN_POINT ( 'NONE',  ( 30.77500000054621765, 17.63344945572770328, 83.50966788445364841 ) ) ;
#9808 = AXIS2_PLACEMENT_3D ( 'NONE', #5648, #8437, #11476 ) ;
#9809 = CARTESIAN_POINT ( 'NONE',  ( 0.000000000000000000, 0.000000000000000000, 0.000000000000000000 ) ) ;
#9810 = CARTESIAN_POINT ( 'NONE',  ( 8.982292369834492973, 24.44317814053119875, -26.52147360909799545 ) ) ;
#9811 = CARTESIAN_POINT ( 'NONE',  ( -10.00000000000000355, 20.00000000000000355, 69.99999999999998579 ) ) ;
#9812 = VERTEX_POINT ( 'NONE', #3219 ) ;
#9813 = CARTESIAN_POINT ( 'NONE',  ( 27.49999999999999645, 20.00000000000000355, 197.9999999999999716 ) ) ;
#9814 = ORIENTED_EDGE ( 'NONE', *, *, #12427, .F. ) ;
#9815 = CARTESIAN_POINT ( 'NONE',  ( 6.000000000000000000, -2.919948986426538440, -5.057499999999997442 ) ) ;
#9816 = AXIS2_PLACEMENT_3D ( 'NONE', #9418, #4587, #10415 ) ;
#9817 = ORIENTED_EDGE ( 'NONE', *, *, #11552, .T. ) ;
#9818 = AXIS2_PLACEMENT_3D ( 'NONE', #10266, #10324, #9330 ) ;
#9819 = ORIENTED_EDGE ( 'NONE', *, *, #4212, .F. ) ;
#9820 =( BOUNDED_CURVE ( )  B_SPLINE_CURVE ( 2, ( #2554, #10291, #8152, #1550, #12019, #4219, #5359, #11957, #7253, #11002, #1431 ),
 .UNSPECIFIED., .F., .F. ) 
 B_SPLINE_CURVE_WITH_KNOTS ( ( 3, 2, 2, 2, 2, 3 ),
 ( 0.8000000000000000444, 0.8066666666666666430, 0.8133333333333333526, 0.8199999999999999512, 0.8266666666666666607, 0.8333333333333333703 ),
 .UNSPECIFIED. ) 
 CURVE ( )  GEOMETRIC_REPRESENTATION_ITEM ( )  RATIONAL_B_SPLINE_CURVE ( ( 1.000000000000000000, 0.9510565162951535312, 1.000000000000000000, 0.9510565162951535312, 1.000000000000000000, 0.9510565162951535312, 1.000000000000000000, 0.9510565162951535312, 1.000000000000000000, 0.9510565162951535312, 1.000000000000000000 ) ) 
 REPRESENTATION_ITEM ( '' )  );
#9821 = DIRECTION ( 'NONE',  ( -1.000000000000000000, -0.000000000000000000, -0.000000000000000000 ) ) ;
#9822 = CARTESIAN_POINT ( 'NONE',  ( -5.000000000000000888, 0.000000000000000000, 169.9999999999999716 ) ) ;
#9823 = CARTESIAN_POINT ( 'NONE',  ( 9.843890364154358252, 21.77789078299004188, 98.08379766955695800 ) ) ;
#9824 = CARTESIAN_POINT ( 'NONE',  ( 36.99999999999999289, 20.00000000000000355, 83.29316153445364534 ) ) ;
#9825 = AXIS2_PLACEMENT_3D ( 'NONE', #7717, #9686, #11337 ) ;
#9826 = CARTESIAN_POINT ( 'NONE',  ( -4.838879514055022923, 48.69911239754581089, -24.52732196506755713 ) ) ;
#9827 = CARTESIAN_POINT ( 'NONE',  ( 4.935074631655826494, 49.18045323697044324, -20.41191120140011606 ) ) ;
#9828 = CARTESIAN_POINT ( 'NONE',  ( 4.464751531075205726, 28.95392510639267414, -20.52201552506329918 ) ) ;
#9829 = CARTESIAN_POINT ( 'NONE',  ( 43.57500000054623257, 24.28113015263587116, 96.68563167572563088 ) ) ;
#9830 = DIRECTION ( 'NONE',  ( -0.000000000000000000, 1.039664082171044875E-15, 1.000000000000000000 ) ) ;
#9831 = ORIENTED_EDGE ( 'NONE', *, *, #9586, .T. ) ;
#9832 = DIRECTION ( 'NONE',  ( -0.7071067811865386910, 8.659560562355043792E-17, -0.7071067811865564545 ) ) ;
#9833 = PRODUCT_CONTEXT ( 'NONE', #2215, 'mechanical' ) ;
#9834 = AXIS2_PLACEMENT_3D ( 'NONE', #552, #11203, #1504 ) ;
#9835 = EDGE_CURVE ( 'NONE', #1690, #2848, #5945, .T. ) ;
#9836 = CARTESIAN_POINT ( 'NONE',  ( 0.000000000000000000, -2.919948986426523341, 5.057500000000002771 ) ) ;
#9837 = DIRECTION ( 'NONE',  ( -1.000000000000000000, -0.000000000000000000, -0.000000000000000000 ) ) ;
#9838 = CARTESIAN_POINT ( 'NONE',  ( 35.77500000054622831, 20.00000000000000355, 98.07665518445361386 ) ) ;
#9839 = CARTESIAN_POINT ( 'NONE',  ( 23.37500000054621907, 27.65831843345427998, 90.79316153445363113 ) ) ;
#9840 = CARTESIAN_POINT ( 'NONE',  ( 24.49999999999998934, 12.11403331821300533, 90.79316153445363113 ) ) ;
#9841 = CARTESIAN_POINT ( 'NONE',  ( 49.59999999999999432, 27.13292387221364876, 93.11078899226573924 ) ) ;
#9842 = CARTESIAN_POINT ( 'NONE',  ( 33.67500000054623399, 22.36655054427230027, 98.07665518445361386 ) ) ;
#9843 = ORIENTED_EDGE ( 'NONE', *, *, #1774, .F. ) ;
#9844 = DIRECTION ( 'NONE',  ( -0.000000000000000000, -0.000000000000000000, 1.000000000000000000 ) ) ;
#9845 = DIRECTION ( 'NONE',  ( 1.000000000000000000, 0.000000000000000000, 0.000000000000000000 ) ) ;
#9846 = ORIENTED_EDGE ( 'NONE', *, *, #5834, .F. ) ;
#9847 = CARTESIAN_POINT ( 'NONE',  ( 1.297896323713631617, 54.83982511471705834, 27.97176989401758362 ) ) ;
#9848 = VERTEX_POINT ( 'NONE', #8797 ) ;
#9849 = CARTESIAN_POINT ( 'NONE',  ( -3.307156092220256749, 53.76411647547837447, -24.78137765757908895 ) ) ;
#9850 = CARTESIAN_POINT ( 'NONE',  ( 6.000000000000000000, 0.000000000000000000, 0.000000000000000000 ) ) ;
#9851 = CARTESIAN_POINT ( 'NONE',  ( 36.97500000054622404, 22.36655054427230382, 83.50966788445364841 ) ) ;
#9852 = FACE_OUTER_BOUND ( 'NONE', #8149, .T. ) ;
#9853 = CARTESIAN_POINT ( 'NONE',  ( 49.47500000054621694, 26.19570976099943849, 95.29460816699764791 ) ) ;
#9854 = CARTESIAN_POINT ( 'NONE',  ( 41.57500000054622546, 26.19570976099943493, 95.29460816699764791 ) ) ;
#9855 = CARTESIAN_POINT ( 'NONE',  ( 42.39999999999998437, 12.86707612778636012, 93.11078899226572503 ) ) ;
#9856 = ADVANCED_FACE ( 'NONE', ( #115 ), #3086, .T. ) ;
#9857 = ADVANCED_FACE ( 'NONE', ( #11847 ), #1133, .T. ) ;
#9858 = DIRECTION ( 'NONE',  ( -0.000000000000000000, -0.000000000000000000, 1.000000000000000000 ) ) ;
#9859 = LINE ( 'NONE', #5862, #5249 ) ;
#9860 = ORIENTED_EDGE ( 'NONE', *, *, #10791, .T. ) ;
#9861 = CARTESIAN_POINT ( 'NONE',  ( 31.05000000109246372, 27.13292387221364876, 88.47553407664153724 ) ) ;
#9862 = CARTESIAN_POINT ( 'NONE',  ( 0.000000000000000000, 20.00000000000000355, -70.00000000000000000 ) ) ;
#9863 = EDGE_LOOP ( 'NONE', ( #6098, #8672, #11240, #11939, #11717, #2816 ) ) ;
#9864 = EDGE_CURVE ( 'NONE', #652, #12355, #3725, .T. ) ;
#9865 = EDGE_LOOP ( 'NONE', ( #2321, #12447, #9130, #3744 ) ) ;
#9866 = DIRECTION ( 'NONE',  ( 0.000000000000000000, 0.000000000000000000, -1.000000000000000000 ) ) ;
#9867 = CARTESIAN_POINT ( 'NONE',  ( 5.000000000000000000, -2.342598717236902051, 4.057500000000004547 ) ) ;
#9868 = CARTESIAN_POINT ( 'NONE',  ( -36.00000000000001421, 77.00000000000000000, 154.3533255156881978 ) ) ;
#9869 = EDGE_CURVE ( 'NONE', #2004, #2031, #5040, .T. ) ;
#9870 = CARTESIAN_POINT ( 'NONE',  ( 31.87500000054622973, 17.63344945572769973, 98.07665518445361386 ) ) ;
#9871 = CARTESIAN_POINT ( 'NONE',  ( 32.07500000054622546, 15.71886984736413417, 96.68563167572563088 ) ) ;
#9872 = CARTESIAN_POINT ( 'NONE',  ( -1.300368161224497943, 54.83901424438912642, 27.97162986671915874 ) ) ;
#9873 = CARTESIAN_POINT ( 'NONE',  ( 6.847974502850965983, 27.29450679136124691, -27.15070937874627788 ) ) ;
#9874 = FACE_OUTER_BOUND ( 'NONE', #10530, .T. ) ;
#9875 = ORIENTED_EDGE ( 'NONE', *, *, #475, .T. ) ;
#9876 = CARTESIAN_POINT ( 'NONE',  ( 0.6578411763953998515, 54.96743791211429908, -24.99342793576595767 ) ) ;
#9877 = ORIENTED_EDGE ( 'NONE', *, *, #6134, .T. ) ;
#9878 = DIRECTION ( 'NONE',  ( 0.000000000000000000, 1.000000000000000000, 0.000000000000000000 ) ) ;
#9879 = EDGE_CURVE ( 'NONE', #8345, #6574, #6904, .T. ) ;
#9880 = ORIENTED_EDGE ( 'NONE', *, *, #2298, .T. ) ;
#9881 = VECTOR ( 'NONE', #4614, 1000.000000000000000 ) ;
#9882 = LINE ( 'NONE', #8211, #7180 ) ;
#9883 = CARTESIAN_POINT ( 'NONE',  ( -9.916489090768509485, 18.66787674250353390, -18.51120417158414000 ) ) ;
#9884 = UNCERTAINTY_MEASURE_WITH_UNIT (LENGTH_MEASURE( 1.000000000000000082E-05 ), #2929, 'distance_accuracy_value', 'NONE');
#9885 = FACE_OUTER_BOUND ( 'NONE', #9049, .T. ) ;
#9886 = CARTESIAN_POINT ( 'NONE',  ( 4.000000000000000000, 20.00000000000000355, 189.9999999999999716 ) ) ;
#9887 = CARTESIAN_POINT ( 'NONE',  ( 27.50000000000000355, 27.49999999999999645, 145.0000000000000000 ) ) ;
#9888 = CARTESIAN_POINT ( 'NONE',  ( 49.99999999999998579, 0.000000000000000000, 169.9999999999999716 ) ) ;
#9889 = CARTESIAN_POINT ( 'NONE',  ( 0.3302971441079701753, 30.00000000000001776, 21.00000000000000711 ) ) ;
#9890 = CARTESIAN_POINT ( 'NONE',  ( -4.493221811708316693, 52.21748163326066106, 20.51407716484954236 ) ) ;
#9891 = DIRECTION ( 'NONE',  ( 0.000000000000000000, 0.000000000000000000, -1.000000000000000000 ) ) ;
#9892 = CARTESIAN_POINT ( 'NONE',  ( 40.77500000054622831, 20.00000000000000355, 83.50966788445364841 ) ) ;
#9893 = CARTESIAN_POINT ( 'NONE',  ( -4.329834338986901621, 47.49413952373966197, -24.62232128246942509 ) ) ;
#9894 = ORIENTED_EDGE ( 'NONE', *, *, #2271, .F. ) ;
#9895 = VECTOR ( 'NONE', #1671, 1000.000000000000000 ) ;
#9896 = CARTESIAN_POINT ( 'NONE',  ( 8.484924050289805564, 25.30202893790023921, -23.51686326738786192 ) ) ;
#9897 = CONTEXT_DEPENDENT_SHAPE_REPRESENTATION ( #4318, #2254 ) ;
#9898 = CARTESIAN_POINT ( 'NONE',  ( 23.37500000054621907, 27.65831843345427998, 90.79316153445363113 ) ) ;
#9899 = FACE_OUTER_BOUND ( 'NONE', #3873, .T. ) ;
#9900 = CARTESIAN_POINT ( 'NONE',  ( 31.97500000054623470, 15.71886984736413417, 96.68563167572563088 ) ) ;
#9901 = CIRCLE ( 'NONE', #4021, 25.00000000000000000 ) ;
#9902 = CARTESIAN_POINT ( 'NONE',  ( 7.537524037383855458, 13.39612119810769819, -23.84148986838564710 ) ) ;
#9903 = CARTESIAN_POINT ( 'NONE',  ( 23.29999999999999005, 26.37988106264029398, 86.15790661882942914 ) ) ;
#9904 = DIRECTION ( 'NONE',  ( 0.000000000000000000, 0.4999999999999984457, -0.8660254037844394848 ) ) ;
#9905 = CARTESIAN_POINT ( 'NONE',  ( 26.27500000054622475, 12.34168156654572535, 90.79316153445363113 ) ) ;
#9906 = ORIENTED_EDGE ( 'NONE', *, *, #2513, .F. ) ;
#9907 = CARTESIAN_POINT ( 'NONE',  ( 0.000000000000000000, 18.00000000000000355, 169.9999999999999716 ) ) ;
#9908 = ORIENTED_EDGE ( 'NONE', *, *, #11166, .T. ) ;
#9909 = EDGE_CURVE ( 'NONE', #2928, #5913, #5960, .T. ) ;
#9910 = DIRECTION ( 'NONE',  ( 1.000000000000000000, 0.000000000000000000, 0.000000000000000000 ) ) ;
#9911 = EDGE_LOOP ( 'NONE', ( #11100, #5528 ) ) ;
#9912 = SHAPE_REPRESENTATION_RELATIONSHIP ( 'NONE' , 'NONE' ,  #4339, #12311 ) ;
#9913 = PRESENTATION_LAYER_ASSIGNMENT (  '', '', ( #6059 ) ) ;
#9914 = FACE_BOUND ( 'NONE', #10346, .T. ) ;
#9915 = CARTESIAN_POINT ( 'NONE',  ( 36.37500000054622973, 12.34168156654572357, 90.79316153445363113 ) ) ;
#9916 = CARTESIAN_POINT ( 'NONE',  ( 12.00000000000000355, 1.102182119232617714E-15, -9.000000000000000000 ) ) ;
#9917 = CYLINDRICAL_SURFACE ( 'NONE', #8809, 7.499999999999992895 ) ;
#9918 = CARTESIAN_POINT ( 'NONE',  ( 41.37500000054622973, 27.65831843345427998, 90.79316153445363113 ) ) ;
#9919 = CARTESIAN_POINT ( 'NONE',  ( 39.49999999999997158, 27.88596668178699645, 90.79316153445363113 ) ) ;
#9920 = CARTESIAN_POINT ( 'NONE',  ( 47.57500000054622546, 24.28113015263587116, 96.68563167572563088 ) ) ;
#9921 = VECTOR ( 'NONE', #3724, 1000.000000000000000 ) ;
#9922 = ORIENTED_EDGE ( 'NONE', *, *, #10633, .F. ) ;
#9923 = CARTESIAN_POINT ( 'NONE',  ( 30.35000000109246088, 13.62011893735971135, 86.15790661882942914 ) ) ;
#9924 = CARTESIAN_POINT ( 'NONE',  ( -1.652347697333065968, 10.13198208422932467, 24.94742907234073215 ) ) ;
#9925 = ORIENTED_EDGE ( 'NONE', *, *, #8701, .F. ) ;
#9926 = DIRECTION ( 'NONE',  ( 0.000000000000000000, 0.5000000000000011102, 0.8660254037844379305 ) ) ;
#9927 = ORIENTED_EDGE ( 'NONE', *, *, #5383, .F. ) ;
#9928 = CARTESIAN_POINT ( 'NONE',  ( -2.000000000000015543, 20.00000000000000355, 90.79316153445363113 ) ) ;
#9929 = EDGE_CURVE ( 'NONE', #1996, #5802, #8164, .T. ) ;
#9930 = CARTESIAN_POINT ( 'NONE',  ( 5.000000000000000000, 50.00000000000000000, -28.00000000000000711 ) ) ;
#9931 = CARTESIAN_POINT ( 'NONE',  ( -2.000000000000015543, 20.00000000000000355, 98.29316153445363113 ) ) ;
#9932 = PRODUCT_DEFINITION_CONTEXT ( 'detailed design', #8052, 'design' ) ;
#9933 = CARTESIAN_POINT ( 'NONE',  ( 29.37500000054622973, 26.92701409722686634, 93.04388485072563242 ) ) ;
#9934 = CARTESIAN_POINT ( 'NONE',  ( 29.57500000054621836, 26.19570976099943493, 95.29460816699764791 ) ) ;
#9935 = EDGE_CURVE ( 'NONE', #2202, #8129, #4590, .T. ) ;
#9936 = CARTESIAN_POINT ( 'NONE',  ( 44.55000000109245661, 17.56310227825322912, 83.29316153445361692 ) ) ;
#9937 = LINE ( 'NONE', #2123, #379 ) ;
#9938 = ORIENTED_EDGE ( 'NONE', *, *, #7673, .F. ) ;
#9939 = CARTESIAN_POINT ( 'NONE',  ( 47.77500000054622120, 22.36655054427230027, 98.07665518445361386 ) ) ;
#9940 = CARTESIAN_POINT ( 'NONE',  ( 49.15000000109245804, 27.88596668178699645, 90.79316153445363113 ) ) ;
#9941 = VERTEX_POINT ( 'NONE', #2343 ) ;
#9942 = CARTESIAN_POINT ( 'NONE',  ( 30.55000000109246372, 17.56310227825320425, 83.29316153445363113 ) ) ;
#9943 = VECTOR ( 'NONE', #5541, 1000.000000000000000 ) ;
#9944 = VERTEX_POINT ( 'NONE', #10260 ) ;
#9945 = CARTESIAN_POINT ( 'NONE',  ( -7.924078669757784965, 13.89146999950097161, -19.44885958033332329 ) ) ;
#9946 = DIRECTION ( 'NONE',  ( -0.000000000000000000, -0.000000000000000000, 1.000000000000000000 ) ) ;
#9947 = VECTOR ( 'NONE', #11920, 1000.000000000000000 ) ;
#9948 = CARTESIAN_POINT ( 'NONE',  ( 1.295572856795887295, 54.84026084924703071, 24.96846459459551681 ) ) ;
#9949 = PRODUCT_DEFINITION_SHAPE ( 'NONE', 'NONE',  #5438 ) ;
#9950 = ADVANCED_FACE ( 'NONE', ( #11278 ), #5203, .F. ) ;
#9951 = CARTESIAN_POINT ( 'NONE',  ( 8.035510277249453992, 25.96172493762885480, 86.21852126538452410 ) ) ;
#9952 = CARTESIAN_POINT ( 'NONE',  ( 49.99999999999998579, 0.000000000000000000, 169.9999999999999716 ) ) ;
#9953 = CARTESIAN_POINT ( 'NONE',  ( 8.481018271693534061, 25.30809127690124782, 19.21224764554878917 ) ) ;
#9954 = DIRECTION ( 'NONE',  ( 0.000000000000000000, 0.000000000000000000, -1.000000000000000000 ) ) ;
#9955 = CARTESIAN_POINT ( 'NONE',  ( 53.99999999999999289, 20.00000000000000711, 189.9999999999999716 ) ) ;
#9956 = B_SPLINE_CURVE_WITH_KNOTS ( 'NONE', 3,
 ( #7226, #11037, #4307, #2347, #4431, #5267, #3356, #1517, #5394, #9266, #445, #3541, #566, #9327, #10151, #6215, #3480, #1462, #629, #7413, #8309, #10322, #1580, #12177, #10088, #10264, #4249, #5459, #2528, #11096, #7347, #9076, #11217, #5207, #4494, #2589, #385, #8121, #2403, #11991, #3295, #7159, #6639, #1698, #8430, #1885, #11406, #11533 ),
 .UNSPECIFIED., .F., .F.,
 ( 4, 2, 2, 2, 2, 2, 2, 2, 2, 2, 2, 2, 2, 2, 2, 2, 2, 2, 2, 2, 2, 2, 2, 4 ),
 ( 3.469446951953614189E-18, 0.001535279795446541822, 0.002302919693169815877, 0.003070559590893089715, 0.003838199488616363120, 0.004605839386339637825, 0.006141119181786200247, 0.007676398977232760067, 0.009211678772679319019, 0.009979318670402598929, 0.01074695856812587884, 0.01151459846584915875, 0.01228223836357244039, 0.01304987826129572030, 0.01381751815901900195, 0.01458515805674228012, 0.01535279795446556003, 0.01688807774991211985, 0.01842335754535867967, 0.01995863734080524296, 0.02149391713625179931, 0.02226155703397508789, 0.02302919693169837301, 0.02456447672714493283 ),
 .UNSPECIFIED. ) ;
#9957 = CARTESIAN_POINT ( 'NONE',  ( 43.17500000054622689, 26.92701409722686634, 88.54243821818162985 ) ) ;
#9958 = CARTESIAN_POINT ( 'NONE',  ( 1.766134315194576754, 45.31947902013321539, 20.92614565884721145 ) ) ;
#9959 = VERTEX_POINT ( 'NONE', #11093 ) ;
#9960 = ADVANCED_FACE ( 'NONE', ( #10085 ), #1397, .F. ) ;
#9961 = VECTOR ( 'NONE', #12123, 1000.000000000000114 ) ;
#9962 = CARTESIAN_POINT ( 'NONE',  ( -3.306342958134543153, 53.76488593550792672, 24.78149064010515445 ) ) ;
#9963 = CARTESIAN_POINT ( 'NONE',  ( 22.17500000054622333, 13.80429023900056507, 95.29460816699764791 ) ) ;
#9964 = CARTESIAN_POINT ( 'NONE',  ( 44.47500000054622404, 13.07298590277314432, 88.54243821818161564 ) ) ;
#9965 = CARTESIAN_POINT ( 'NONE',  ( 33.37500000054622973, 26.92701409722686634, 93.04388485072563242 ) ) ;
#9966 = CARTESIAN_POINT ( 'NONE',  ( 21.47500000054622404, 26.92701409722686634, 93.04388485072563242 ) ) ;
#9967 = CARTESIAN_POINT ( 'NONE',  ( 21.29999999999999005, 26.37988106264029398, 86.15790661882942914 ) ) ;
#9968 = CARTESIAN_POINT ( 'NONE',  ( 28.57500000054622902, 15.71886984736413773, 84.90069139318163138 ) ) ;
#9969 = VERTEX_POINT ( 'NONE', #5264 ) ;
#9970 = CARTESIAN_POINT ( 'NONE',  ( 4.999999999999999112, 0.000000000000000000, 169.9999999999999716 ) ) ;
#9971 = VERTEX_POINT ( 'NONE', #381 ) ;
#9972 = ORIENTED_EDGE ( 'NONE', *, *, #10107, .T. ) ;
#9973 = CARTESIAN_POINT ( 'NONE',  ( 6.000000000000000000, 2.919948986426538884, 5.057499999999996554 ) ) ;
#9974 = ORIENTED_EDGE ( 'NONE', *, *, #3645, .T. ) ;
#9975 = CARTESIAN_POINT ( 'NONE',  ( 0.000000000000000000, 22.00000000000000000, 169.9999999999999716 ) ) ;
#9976 = CARTESIAN_POINT ( 'NONE',  ( 38.47500000054622404, 13.07298590277314432, 88.54243821818161564 ) ) ;
#9977 = CARTESIAN_POINT ( 'NONE',  ( -3.307119090283400897, 53.76412354891344592, -27.80497456210996887 ) ) ;
#9978 = EDGE_CURVE ( 'NONE', #5913, #11430, #4304, .T. ) ;
#9979 = CARTESIAN_POINT ( 'NONE',  ( 19.95000000109246230, 13.62011893735970958, 95.42841645007781892 ) ) ;
#9980 = CARTESIAN_POINT ( 'NONE',  ( 41.77500000054621410, 22.36655054427230027, 98.07665518445361386 ) ) ;
#9981 = CARTESIAN_POINT ( 'NONE',  ( 44.49999999999999289, 12.11403331821300533, 90.79316153445363113 ) ) ;
#9982 = CARTESIAN_POINT ( 'NONE',  ( 46.57500000054622546, 15.71886984736413773, 84.90069139318163138 ) ) ;
#9983 = ORIENTED_EDGE ( 'NONE', *, *, #11531, .F. ) ;
#9984 = CARTESIAN_POINT ( 'NONE',  ( 27.65000000109246514, 20.00000000000000355, 98.29316153445363113 ) ) ;
#9985 = CARTESIAN_POINT ( 'NONE',  ( -10.00000000000000355, 20.00000000000000355, -66.99999999999998579 ) ) ;
#9986 = ORIENTED_EDGE ( 'NONE', *, *, #9086, .T. ) ;
#9987 = CARTESIAN_POINT ( 'NONE',  ( 4.967692037346607137, 50.65500470054040250, -20.40407670487946135 ) ) ;
#9988 = ORIENTED_EDGE ( 'NONE', *, *, #391, .T. ) ;
#9989 = DIRECTION ( 'NONE',  ( -0.000000000000000000, -0.000000000000000000, 1.000000000000000000 ) ) ;
#9990 = CARTESIAN_POINT ( 'NONE',  ( 41.55000000109246372, 22.43689772174679575, 98.29316153445363113 ) ) ;
#9991 = CARTESIAN_POINT ( 'NONE',  ( 48.79999999999999005, 15.59161060780646046, 84.72553407664153724 ) ) ;
#9992 = EDGE_CURVE ( 'NONE', #513, #11209, #563, .T. ) ;
#9993 = CARTESIAN_POINT ( 'NONE',  ( 33.67500000054623399, 22.36655054427230027, 98.07665518445361386 ) ) ;
#9994 = CARTESIAN_POINT ( 'NONE',  ( 32.97500000054621694, 22.36655054427230382, 83.50966788445364841 ) ) ;
#9995 = APPLICATION_CONTEXT ( 'automotive_design' ) ;
#9996 = VECTOR ( 'NONE', #1274, 1000.000000000000000 ) ;
#9997 = CARTESIAN_POINT ( 'NONE',  ( 49.99999999999998579, 20.00000000000000355, 98.29316153445363113 ) ) ;
#9998 = CARTESIAN_POINT ( 'NONE',  ( 9.353276081244219498, 23.55311451265283296, 23.18479875781715194 ) ) ;
#9999 = DIRECTION ( 'NONE',  ( -1.000000000000000000, 0.000000000000000000, 0.000000000000000000 ) ) ;
#10000 = ORIENTED_EDGE ( 'NONE', *, *, #8828, .F. ) ;
#10001 = ADVANCED_FACE ( 'NONE', ( #10147 ), #348, .T. ) ;
#10002 = CARTESIAN_POINT ( 'NONE',  ( 41.05000000109246372, 27.13292387221364876, 88.47553407664153724 ) ) ;
#10003 = CARTESIAN_POINT ( 'NONE',  ( -31.74999999999995737, 1.102182119232617714E-15, -9.000000000000000000 ) ) ;
#10004 = ORIENTED_EDGE ( 'NONE', *, *, #3083, .T. ) ;
#10005 = CARTESIAN_POINT ( 'NONE',  ( 45.65000000109247225, 20.00000000000000355, 98.29316153445363113 ) ) ;
#10006 = VERTEX_POINT ( 'NONE', #12053 ) ;
#10007 = CARTESIAN_POINT ( 'NONE',  ( -0.6619244392933834042, 10.00000000000000178, -21.00000000000000711 ) ) ;
#10008 = VECTOR ( 'NONE', #11271, 1000.000000000000000 ) ;
#10009 = PRODUCT_DEFINITION_FORMATION_WITH_SPECIFIED_SOURCE ( 'ANY', '', #10963, .NOT_KNOWN. ) ;
#10010 = FACE_OUTER_BOUND ( 'NONE', #2678, .T. ) ;
#10011 = CARTESIAN_POINT ( 'NONE',  ( 10.00000000000000355, 20.25957311745080958, 83.29316153445364534 ) ) ;
#10012 = PLANE ( 'NONE',  #2402 ) ;
#10013 = SHAPE_REPRESENTATION ( 'Bearing', ( #9021 ), #2935 ) ;
#10015 = EDGE_CURVE ( 'NONE', #8158, #9799, #3353, .T. ) ;
#10014 = VECTOR ( 'NONE', #4981, 1000.000000000000000 ) ;
#10016 = CARTESIAN_POINT ( 'NONE',  ( 6.955575927950914131E-22, 45.00000000000000711, -25.00000000000000000 ) ) ;
#10017 = CARTESIAN_POINT ( 'NONE',  ( 2.559760333650129958E-15, 55.00000000000000000, 21.00000000000000000 ) ) ;
#10018 = CARTESIAN_POINT ( 'NONE',  ( -1.609496042995007370, 45.26329109710995624, 27.95414474166305041 ) ) ;
#10019 = AXIS2_PLACEMENT_3D ( 'NONE', #1309, #9297, #11070 ) ;
#10020 = CARTESIAN_POINT ( 'NONE',  ( 44.97500000054623115, 24.28113015263587471, 84.90069139318163138 ) ) ;
#10021 = CARTESIAN_POINT ( 'NONE',  ( -31.74999999999995737, 0.000000000000000000, 0.000000000000000000 ) ) ;
#10022 = EDGE_LOOP ( 'NONE', ( #10890, #968 ) ) ;
#10023 = CARTESIAN_POINT ( 'NONE',  ( -9.983620353272891990, 19.33838559509563026, -26.15967447858658090 ) ) ;
#10024 = EDGE_CURVE ( 'NONE', #9272, #1221, #2318, .T. ) ;
#10025 = AXIS2_PLACEMENT_3D ( 'NONE', #1483, #2429, #4996 ) ;
#10026 = CARTESIAN_POINT ( 'NONE',  ( 4.967437465254620932, 50.65784153438875848, 24.50160996501502098 ) ) ;
#10027 = CARTESIAN_POINT ( 'NONE',  ( 46.77500000054622831, 17.63344945572770328, 83.50966788445364841 ) ) ;
#10028 = CARTESIAN_POINT ( 'NONE',  ( 31.57500000054622902, 24.28113015263587116, 96.68563167572563088 ) ) ;
#10029 = EDGE_CURVE ( 'NONE', #6345, #4797, #9460, .T. ) ;
#10030 = CARTESIAN_POINT ( 'NONE',  ( 23.17500000054622689, 26.19570976099943493, 86.29171490190961435 ) ) ;
#10031 = CYLINDRICAL_SURFACE ( 'NONE', #3591, 5.000000000000000000 ) ;
#10032 = PLANE ( 'NONE',  #1413 ) ;
#10033 = CARTESIAN_POINT ( 'NONE',  ( 26.17500000054623044, 13.07298590277314254, 93.04388485072563242 ) ) ;
#10034 = ORIENTED_EDGE ( 'NONE', *, *, #8425, .F. ) ;
#10035 = CARTESIAN_POINT ( 'NONE',  ( 22.85000000109246443, 24.40838939219355197, 84.72553407664153724 ) ) ;
#10036 = ORIENTED_EDGE ( 'NONE', *, *, #302, .F. ) ;
#10037 = ORIENTED_EDGE ( 'NONE', *, *, #4697, .T. ) ;
#10038 = CARTESIAN_POINT ( 'NONE',  ( 38.19999999999998863, 15.59161060780645691, 96.86078899226572503 ) ) ;
#10039 = ORIENTED_EDGE ( 'NONE', *, *, #3789, .T. ) ;
#10040 = DIRECTION ( 'NONE',  ( 1.000000000000000000, 0.000000000000000000, 0.000000000000000000 ) ) ;
#10041 = AXIS2_PLACEMENT_3D ( 'NONE', #1798, #11507, #2817 ) ;
#10042 = CARTESIAN_POINT ( 'NONE',  ( 37.87500000054622262, 20.00000000000000355, 98.07665518445361386 ) ) ;
#10043 = CARTESIAN_POINT ( 'NONE',  ( 36.99999999999999289, 20.00000000000000355, 83.29316153445364534 ) ) ;
#10044 = CARTESIAN_POINT ( 'NONE',  ( 26.29999999999998295, 13.62011893735970958, 95.42841645007781892 ) ) ;
#10045 = CARTESIAN_POINT ( 'NONE',  ( 41.07500000054622546, 24.28113015263587471, 84.90069139318163138 ) ) ;
#10046 = CARTESIAN_POINT ( 'NONE',  ( 36.79999999999998295, 15.59161060780646046, 84.72553407664153724 ) ) ;
#10047 = CIRCLE ( 'NONE', #3948, 4.171999999999999709 ) ;
#10048 = CARTESIAN_POINT ( 'NONE',  ( 43.87500000054622973, 17.63344945572769973, 98.07665518445361386 ) ) ;
#10049 = EDGE_LOOP ( 'NONE', ( #10034, #5943 ) ) ;
#10050 = CARTESIAN_POINT ( 'NONE',  ( 22.95000000109246230, 26.37988106264029398, 86.15790661882942914 ) ) ;
#10051 = DIRECTION ( 'NONE',  ( 0.000000000000000000, 0.000000000000000000, 1.000000000000000000 ) ) ;
#10052 = ORIENTED_EDGE ( 'NONE', *, *, #4424, .T. ) ;
#10053 = CARTESIAN_POINT ( 'NONE',  ( -9.983885927020196505, 20.65630489035274664, 26.15957239041219395 ) ) ;
#10054 = ORIENTED_EDGE ( 'NONE', *, *, #8294, .F. ) ;
#10055 = DIRECTION ( 'NONE',  ( 1.000000000000000000, -0.000000000000000000, -0.000000000000000000 ) ) ;
#10056 = PRODUCT_DEFINITION_SHAPE ( 'NONE', 'NONE',  #10161 ) ;
#10057 = CARTESIAN_POINT ( 'NONE',  ( 5.000000000000000000, 50.00000000000000000, -27.54995462791182703 ) ) ;
#10058 = CARTESIAN_POINT ( 'NONE',  ( 12.59999999999999964, 7.347880794884123680E-16, -6.000000000000003553 ) ) ;
#10059 = CARTESIAN_POINT ( 'NONE',  ( 27.67500000054623044, 22.36655054427230027, 98.07665518445361386 ) ) ;
#10060 = CARTESIAN_POINT ( 'NONE',  ( 28.27500000054622475, 13.07298590277314254, 93.04388485072563242 ) ) ;
#10061 = CARTESIAN_POINT ( 'NONE',  ( 3.543374587579615209, 29.35684306698988877, 27.77654735269002018 ) ) ;
#10062 = DIRECTION ( 'NONE',  ( -0.000000000000000000, -1.000000000000000000, -0.000000000000000000 ) ) ;
#10063 = ORIENTED_EDGE ( 'NONE', *, *, #12193, .T. ) ;
#10064 = CARTESIAN_POINT ( 'NONE',  ( 42.75000000109245946, 22.43689772174679575, 83.29316153445363113 ) ) ;
#10065 = SURFACE_STYLE_USAGE ( .BOTH. , #4284 ) ;
#10066 = VERTEX_POINT ( 'NONE', #1694 ) ;
#10067 = CARTESIAN_POINT ( 'NONE',  ( 32.65000000109246514, 20.00000000000000355, 83.29316153445364534 ) ) ;
#10068 = VERTEX_POINT ( 'NONE', #7600 ) ;
#10069 = EDGE_CURVE ( 'NONE', #2755, #2485, #4398, .T. ) ;
#10070 = CARTESIAN_POINT ( 'NONE',  ( -9.655198859856366056, 17.37602299191694044, -18.64909941108382796 ) ) ;
#10071 = VECTOR ( 'NONE', #6890, 1000.000000000000000 ) ;
#10072 = DIRECTION ( 'NONE',  ( 0.000000000000000000, 0.000000000000000000, 1.000000000000000000 ) ) ;
#10073 = ADVANCED_FACE ( 'NONE', ( #810 ), #10380, .F. ) ;
#10074 = DIRECTION ( 'NONE',  ( 1.000000000000000000, 0.000000000000000000, 0.000000000000000000 ) ) ;
#10075 = LINE ( 'NONE', #11084, #11729 ) ;
#10076 = CARTESIAN_POINT ( 'NONE',  ( -0.6688742877673069520, 10.01682275176732162, 20.99197381862867928 ) ) ;
#10077 = CARTESIAN_POINT ( 'NONE',  ( -50.00000000000001421, 0.000000000000000000, 169.9999999999999716 ) ) ;
#10078 = VECTOR ( 'NONE', #6767, 1000.000000000000000 ) ;
#10079 = CARTESIAN_POINT ( 'NONE',  ( 6.119244668491610639, 27.93539859446131501, -20.09633498124250295 ) ) ;
#10080 = DIRECTION ( 'NONE',  ( -0.000000000000000000, -0.000000000000000000, 1.000000000000000000 ) ) ;
#10081 = VERTEX_POINT ( 'NONE', #11346 ) ;
#10082 = CARTESIAN_POINT ( 'NONE',  ( -4.968274749745848595, 50.65218571871033504, 24.50144017370611493 ) ) ;
#10083 = CARTESIAN_POINT ( 'NONE',  ( 10.00000000000000178, 19.67085183536559967, -26.15339366124404208 ) ) ;
#10084 = EDGE_CURVE ( 'NONE', #1716, #6066, #4682, .T. ) ;
#10085 = FACE_OUTER_BOUND ( 'NONE', #7724, .T. ) ;
#10086 = CARTESIAN_POINT ( 'NONE',  ( 43.27500000054622120, 26.92701409722686634, 88.54243821818162985 ) ) ;
#10087 = CARTESIAN_POINT ( 'NONE',  ( 25.37500000054622973, 26.92701409722686634, 93.04388485072563242 ) ) ;
#10088 = CARTESIAN_POINT ( 'NONE',  ( 6.614382007193625235, 12.50000328913819381, 90.53699374271461409 ) ) ;
#10089 = DIRECTION ( 'NONE',  ( 0.000000000000000000, 0.000000000000000000, 1.000000000000000000 ) ) ;
#10090 = DIRECTION ( 'NONE',  ( 0.000000000000000000, 0.000000000000000000, -1.000000000000000000 ) ) ;
#10091 = CARTESIAN_POINT ( 'NONE',  ( 6.000000000000000000, 5.839897972853064445, -8.673617379884035472E-15 ) ) ;
#10092 = CARTESIAN_POINT ( 'NONE',  ( 29.77500000054622831, 20.00000000000000355, 98.07665518445361386 ) ) ;
#10093 = ORIENTED_EDGE ( 'NONE', *, *, #1575, .T. ) ;
#10094 = FACE_OUTER_BOUND ( 'NONE', #4272, .T. ) ;
#10095 = ORIENTED_EDGE ( 'NONE', *, *, #10182, .T. ) ;
#10096 = DIRECTION ( 'NONE',  ( 1.000000000000000000, 0.000000000000000000, 0.000000000000000000 ) ) ;
#10097 = ORIENTED_EDGE ( 'NONE', *, *, #2722, .F. ) ;
#10098 =( NAMED_UNIT ( * ) SI_UNIT ( $, .STERADIAN. ) SOLID_ANGLE_UNIT ( ) );
#10099 = EDGE_CURVE ( 'NONE', #1748, #9751, #3784, .T. ) ;
#10100 = VECTOR ( 'NONE', #6375, 1000.000000000000000 ) ;
#10101 = CARTESIAN_POINT ( 'NONE',  ( 29.47500000054622404, 26.92701409722686634, 93.04388485072563242 ) ) ;
#10102 = CARTESIAN_POINT ( 'NONE',  ( -5.000000000000004441, 20.00000000000000000, 145.0000000000000000 ) ) ;
#10103 = CARTESIAN_POINT ( 'NONE',  ( 46.07500000054622546, 13.80429023900056507, 95.29460816699764791 ) ) ;
#10104 = CARTESIAN_POINT ( 'NONE',  ( 33.97500000054620983, 17.63344945572769973, 98.07665518445361386 ) ) ;
#10105 = CARTESIAN_POINT ( 'NONE',  ( 35.19999999999998863, 24.40838939219355197, 84.72553407664153724 ) ) ;
#10106 = VECTOR ( 'NONE', #3515, 1000.000000000000000 ) ;
#10107 = EDGE_CURVE ( 'NONE', #7779, #6176, #685, .T. ) ;
#10108 = CARTESIAN_POINT ( 'NONE',  ( 48.87500000054622262, 22.36655054427230382, 83.50966788445364841 ) ) ;
#10109 = VERTEX_POINT ( 'NONE', #6457 ) ;
#10110 = CARTESIAN_POINT ( 'NONE',  ( 21.95000000109245875, 13.62011893735971135, 95.42841645007781892 ) ) ;
#10111 = CARTESIAN_POINT ( 'NONE',  ( -6.609692946276023662, 12.48878433695339218, 24.11181729628509984 ) ) ;
#10112 = ORIENTED_EDGE ( 'NONE', *, *, #5202, .T. ) ;
#10113 = AXIS2_PLACEMENT_3D ( 'NONE', #5949, #2010, #4103 ) ;
#10114 = CARTESIAN_POINT ( 'NONE',  ( 10.00000000000000355, 20.00000000000000355, 22.91287847477919826 ) ) ;
#10115 = VERTEX_POINT ( 'NONE', #12420 ) ;
#10116 = ADVANCED_FACE ( 'NONE', ( #3717 ), #6636, .T. ) ;
#10117 = DIRECTION ( 'NONE',  ( -1.000000000000000000, -0.000000000000000000, -0.000000000000000000 ) ) ;
#10118 = CARTESIAN_POINT ( 'NONE',  ( 21.25000000109246301, 27.13292387221364876, 93.11078899226573924 ) ) ;
#10119 = LINE ( 'NONE', #5298, #8864 ) ;
#10120 = CYLINDRICAL_SURFACE ( 'NONE', #8195, 10.00000000000000355 ) ;
#10121 = CIRCLE ( 'NONE', #6461, 7.499999999999978684 ) ;
#10122 = CARTESIAN_POINT ( 'NONE',  ( 33.57500000054623257, 24.28113015263587116, 96.68563167572563088 ) ) ;
#10123 = CARTESIAN_POINT ( 'NONE',  ( 26.57500000054622191, 13.80429023900056684, 86.29171490190961435 ) ) ;
#10124 = DIRECTION ( 'NONE',  ( -0.000000000000000000, -1.000000000000000000, -0.000000000000000000 ) ) ;
#10125 = VECTOR ( 'NONE', #8351, 1000.000000000000000 ) ;
#10126 = DIRECTION ( 'NONE',  ( -1.000000000000000000, 0.000000000000000000, 0.000000000000000000 ) ) ;
#10127 = VERTEX_POINT ( 'NONE', #10507 ) ;
#10128 = CARTESIAN_POINT ( 'NONE',  ( 45.75000000109246656, 17.56310227825320425, 98.29316153445363113 ) ) ;
#10129 = DIRECTION ( 'NONE',  ( -0.000000000000000000, 1.295896757998781572E-15, 1.000000000000000000 ) ) ;
#10130 = ORIENTED_EDGE ( 'NONE', *, *, #3945, .T. ) ;
#10131 = CARTESIAN_POINT ( 'NONE',  ( 0.000000000000000000, 139.9999999999999716, 0.000000000000000000 ) ) ;
#10132 = EDGE_CURVE ( 'NONE', #9159, #3577, #11488, .T. ) ;
#10133 = ORIENTED_EDGE ( 'NONE', *, *, #11465, .T. ) ;
#10134 = CARTESIAN_POINT ( 'NONE',  ( -9.866849862893351641, 18.34052833014279216, -18.53781888910907938 ) ) ;
#10135 = CARTESIAN_POINT ( 'NONE',  ( 3.061617454482527662E-15, 30.00000000000001066, 25.00000000000000000 ) ) ;
#10136 = DIRECTION ( 'NONE',  ( 0.000000000000000000, 0.000000000000000000, -1.000000000000000000 ) ) ;
#10137 = ADVANCED_FACE ( 'NONE', ( #9570, #5704 ), #2839, .F. ) ;
#10138 = AXIS2_PLACEMENT_3D ( 'NONE', #7747, #5785, #3051 ) ;
#10139 = CARTESIAN_POINT ( 'NONE',  ( -2.306453115620162198, 10.26403383852864870, 20.87548082228511603 ) ) ;
#10140 = DIRECTION ( 'NONE',  ( 1.000000000000000000, 0.000000000000000000, 0.000000000000000000 ) ) ;
#10141 = CARTESIAN_POINT ( 'NONE',  ( 9.353276081244219498, 23.55311451265283296, 23.18479875781715194 ) ) ;
#10142 = CARTESIAN_POINT ( 'NONE',  ( 33.99999999999998579, 20.00000000000000355, 98.29316153445363113 ) ) ;
#10143 = ORIENTED_EDGE ( 'NONE', *, *, #908, .F. ) ;
#10144 = CARTESIAN_POINT ( 'NONE',  ( -9.868592978625752465, 18.35130037890183985, -26.20335131078380897 ) ) ;
#10145 = AXIS2_PLACEMENT_3D ( 'NONE', #2409, #2232, #6221 ) ;
#10146 = DIRECTION ( 'NONE',  ( -1.000000000000000000, 0.000000000000000000, 0.000000000000000000 ) ) ;
#10147 = FACE_OUTER_BOUND ( 'NONE', #12048, .T. ) ;
#10148 = CARTESIAN_POINT ( 'NONE',  ( 41.57500000054622546, 26.19570976099943493, 95.29460816699764791 ) ) ;
#10149 = CARTESIAN_POINT ( 'NONE',  ( 24.17500000054622689, 13.07298590277314254, 93.04388485072563242 ) ) ;
#10150 =( BOUNDED_CURVE ( )  B_SPLINE_CURVE ( 2, ( #7295, #4257, #4378, #331, #4194, #9084, #1410, #8131, #10038, #2292, #2355 ),
 .UNSPECIFIED., .F., .F. ) 
 B_SPLINE_CURVE_WITH_KNOTS ( ( 3, 2, 2, 2, 2, 3 ),
 ( 0.3666666666666666963, 0.3733333333333333504, 0.3799999999999999489, 0.3866666666666666030, 0.3933333333333332016, 0.3999999999999998557 ),
 .UNSPECIFIED. ) 
 CURVE ( )  GEOMETRIC_REPRESENTATION_ITEM ( )  RATIONAL_B_SPLINE_CURVE ( ( 0.9999999999999995559, 0.9510565162951539753, 1.000000000000000000, 0.9510565162951535312, 1.000000000000000000, 0.9510565162951535312, 1.000000000000000000, 0.9510565162951535312, 1.000000000000000000, 0.9510565162951547524, 0.9999999999999987788 ) ) 
 REPRESENTATION_ITEM ( '' )  );
#10151 = CARTESIAN_POINT ( 'NONE',  ( 8.033354630240914673, 14.03538636471792778, 86.22229691711790167 ) ) ;
#10152 = LINE ( 'NONE', #567, #11005 ) ;
#10153 = CARTESIAN_POINT ( 'NONE',  ( 6.000000000000000000, 5.839897972853064445, -8.673617379884035472E-15 ) ) ;
#10154 = FACE_OUTER_BOUND ( 'NONE', #9083, .T. ) ;
#10155 = ORIENTED_EDGE ( 'NONE', *, *, #2996, .F. ) ;
#10156 = VECTOR ( 'NONE', #9473, 1000.000000000000000 ) ;
#10157 = ADVANCED_FACE ( 'NONE', ( #11529 ), #7536, .T. ) ;
#10158 = ORIENTED_EDGE ( 'NONE', *, *, #12049, .F. ) ;
#10159 = CARTESIAN_POINT ( 'NONE',  ( 36.99999999999995026, 40.00000000000000000, 69.99999999999998579 ) ) ;
#10160 = ORIENTED_EDGE ( 'NONE', *, *, #9992, .T. ) ;
#10161 = PRODUCT_DEFINITION ( 'UNKNOWN', '', #10009, #9932 ) ;
#10162 =( REPRESENTATION_RELATIONSHIP ('NONE','NONE', #4262, #10013 ) REPRESENTATION_RELATIONSHIP_WITH_TRANSFORMATION ( #4113 )SHAPE_REPRESENTATION_RELATIONSHIP( ) );
#10163 = CARTESIAN_POINT ( 'NONE',  ( 30.17500000054621978, 13.80429023900056507, 95.29460816699764791 ) ) ;
#10164 = DIRECTION ( 'NONE',  ( 0.000000000000000000, 0.000000000000000000, 1.000000000000000000 ) ) ;
#10165 = CARTESIAN_POINT ( 'NONE',  ( 46.97500000054623115, 24.28113015263587471, 84.90069139318163138 ) ) ;
#10166 = CARTESIAN_POINT ( 'NONE',  ( 34.07500000054622546, 15.71886984736413417, 96.68563167572563088 ) ) ;
#10167 = CARTESIAN_POINT ( 'NONE',  ( 33.59999999999999432, 27.13292387221364876, 93.11078899226573924 ) ) ;
#10168 = CARTESIAN_POINT ( 'NONE',  ( 43.07500000054622546, 26.19570976099943493, 86.29171490190961435 ) ) ;
#10169 = ORIENTED_EDGE ( 'NONE', *, *, #3200, .F. ) ;
#10170 = CARTESIAN_POINT ( 'NONE',  ( 21.85000000109246443, 15.59161060780645691, 96.86078899226572503 ) ) ;
#10171 = CARTESIAN_POINT ( 'NONE',  ( -6.851336394414588860, 12.70864359358585460, 24.04404201862471524 ) ) ;
#10172 = ORIENTED_EDGE ( 'NONE', *, *, #5676, .T. ) ;
#10173 = CARTESIAN_POINT ( 'NONE',  ( -1.322605739864947116, 29.91771837663726785, 27.97070232718573735 ) ) ;
#10174 = ORIENTED_EDGE ( 'NONE', *, *, #100, .F. ) ;
#10175 = CARTESIAN_POINT ( 'NONE',  ( 0.000000000000000000, 139.9999999999999716, -21.00000000000000000 ) ) ;
#10176 = ADVANCED_FACE ( 'NONE', ( #3596 ), #1883, .T. ) ;
#10177 = LINE ( 'NONE', #11067, #288 ) ;
#10178 = CARTESIAN_POINT ( 'NONE',  ( 26.67500000054622689, 17.63344945572770328, 83.50966788445364841 ) ) ;
#10179 = CARTESIAN_POINT ( 'NONE',  ( 25.47500000054622404, 26.92701409722686634, 93.04388485072563242 ) ) ;
#10180 = ADVANCED_FACE ( 'NONE', ( #1635 ), #7646, .T. ) ;
#10181 = CARTESIAN_POINT ( 'NONE',  ( 2.606202220541010028, 29.66002383724781311, 27.88024221855608431 ) ) ;
#10182 = EDGE_CURVE ( 'NONE', #9159, #11119, #9274, .T. ) ;
#10183 = CARTESIAN_POINT ( 'NONE',  ( 1.000000000000000888, 20.00000000000000355, 189.0000000000000000 ) ) ;
#10184 = VERTEX_POINT ( 'NONE', #4552 ) ;
#10185 = CARTESIAN_POINT ( 'NONE',  ( 44.15000000109247225, 12.11403331821300533, 90.79316153445363113 ) ) ;
#10186 = CARTESIAN_POINT ( 'NONE',  ( 45.99999999999998579, 20.00000000000000355, 98.29316153445363113 ) ) ;
#10187 = ORIENTED_EDGE ( 'NONE', *, *, #7882, .T. ) ;
#10188 = DIRECTION ( 'NONE',  ( 1.000000000000000000, -0.000000000000000000, -0.000000000000000000 ) ) ;
#10189 = ORIENTED_EDGE ( 'NONE', *, *, #7470, .F. ) ;
#10190 = CARTESIAN_POINT ( 'NONE',  ( 3.972187451669499936, 53.05441016201150717, 20.62174624516992694 ) ) ;
#10191 = CARTESIAN_POINT ( 'NONE',  ( -1.322864546895947679, 29.91770977471893289, 24.96717945133217498 ) ) ;
#10192 = CARTESIAN_POINT ( 'NONE',  ( 2.571758278209441661E-15, 139.9999999999999716, 21.00000000000000000 ) ) ;
#10193 = AXIS2_PLACEMENT_3D ( 'NONE', #258, #1959, #6905 ) ;
#10194 = CARTESIAN_POINT ( 'NONE',  ( -10.00000000000001066, 19.67111324348436696, 22.91287847477920536 ) ) ;
#10195 = DIRECTION ( 'NONE',  ( -1.000000000000000000, -0.000000000000000000, -0.000000000000000000 ) ) ;
#10196 = CARTESIAN_POINT ( 'NONE',  ( 42.29999999999998295, 13.62011893735970958, 95.42841645007781892 ) ) ;
#10197 = CARTESIAN_POINT ( 'NONE',  ( -9.674627460180301952, 17.38490666077015590, 26.27586073059115535 ) ) ;
#10198 = LINE ( 'NONE', #9255, #12467 ) ;
#10199 = VECTOR ( 'NONE', #6584, 1000.000000000000114 ) ;
#10200 = CARTESIAN_POINT ( 'NONE',  ( 23.89999999999998792, 22.43689772174679575, 98.29316153445363113 ) ) ;
#10201 = ORIENTED_EDGE ( 'NONE', *, *, #3707, .F. ) ;
#10202 = CARTESIAN_POINT ( 'NONE',  ( 2.504881716134078395, 54.33965200799452333, 24.87570091612971979 ) ) ;
#10203 = CARTESIAN_POINT ( 'NONE',  ( 43.17500000054621978, 26.19570976099943493, 86.29171490190961435 ) ) ;
#10204 = VECTOR ( 'NONE', #2637, 1000.000000000000000 ) ;
#10205 = CARTESIAN_POINT ( 'NONE',  ( 28.17500000054622689, 13.07298590277314254, 93.04388485072563242 ) ) ;
#10206 = LINE ( 'NONE', #4372, #1197 ) ;
#10207 = PLANE ( 'NONE',  #10676 ) ;
#10208 = CARTESIAN_POINT ( 'NONE',  ( 33.79999999999999005, 24.40838939219354842, 96.86078899226572503 ) ) ;
#10209 = DIRECTION ( 'NONE',  ( -0.000000000000000000, -0.7071067811865511255, -0.7071067811865440200 ) ) ;
#10210 = EDGE_LOOP ( 'NONE', ( #4439, #8915, #3005, #2162 ) ) ;
#10211 = CARTESIAN_POINT ( 'NONE',  ( 6.000000000000000000, 2.919948986426539772, 5.057499999999996554 ) ) ;
#10212 = VERTEX_POINT ( 'NONE', #2585 ) ;
#10213 = CYLINDRICAL_SURFACE ( 'NONE', #7925, 7.499999999999992895 ) ;
#10214 = EDGE_LOOP ( 'NONE', ( #3886, #4014, #4501 ) ) ;
#10215 = EDGE_CURVE ( 'NONE', #1878, #8530, #4601, .T. ) ;
#10216 = AXIS2_PLACEMENT_3D ( 'NONE', #11317, #3693, #9547 ) ;
#10217 =( BOUNDED_SURFACE ( )  B_SPLINE_SURFACE ( 1, 2, ( 
 ( #10864, #914, #4782, #8647, #12519, #7699, #11566, #3252, #1230, #10108, #7118, #3192, #4386, #12133, #6112, #344, #10930, #7053, #10993, #4207, #402, #2302, #9920, #3441, #7305, #2421, #9158, #2245, #11115, #5099, #6298, #3373, #9982, #11056, #8964, #2363, #11178, #8203, #6047, #1475, #277, #9032, #5287, #4140, #8015, #1419, #11948, #463, #11886, #6171, #6234, #5347, #526, #1291, #5164, #8080, #1358, #4325, #12072, #10048, #5225, #9095, #7243, #4266, #8142, #8264, #12008, #10168, #3311, #9219, #7178, #2735, #6535, #2481, #1538, #1772, #11302, #1715, #6357, #5411, #10403, #8386, #5596, #10224, #2608, #7494, #5657, #9529, #7366, #585, #8570, #10340, #9467, #4635, #4451, #8329, #12441, #11365, #9345, #5538, #4698, #9282, #2672, #3558, #766, #3739, #6594, #8506, #12195, #3495, #828, #6477, #11426, #4511, #1597, #6416, #1657, #9404, #11235, #2544, #12381, #5478, #7431, #10280, #648, #12255, #10462, #7620, #3679, #706, #7557, #4575, #8447, #12316, #3615, #1155, #3933, #1838, #8882, #10715, #8630, #4830, #7745, #5781, #9655, #11742, #7807, #2794, #1964, #9587, #8696, #3049, #5966, #5720, #6910, #8816, #3869, #894, #10777, #9777, #9715, #9842, #4764, #2921, #11613, #5844, #5017, #135, #5, #1030, #6784, #6656, #2986, #10651, #12500, #200, #4056, #11548, #962, #3805, #7684, #4892, #8752, #68, #11680, #10525, #11484, #2859, #7872, #2026, #6720, #3994, #10587, #2090, #1899, #6852, #5909, #1087, #4953, #678, #10092, #5510, #3528, #9377, #10914, #7999, #2159, #8190, #5149, #5271, #1218, #5084, #9968, #2287, #1276, #2229, #3176, #3238, #11871, #2578, #10311, #6158, #9015, #12226, #326, #4252, #9143, #2351, #1630, #3298, #8124, #1406, #7401, #11272, #6976, #9905, #10033, #7936, #7039, #11994, #9079, #449, #6449, #6218, #1342, #11799, #7099, #3107, #10846, #4311, #5209, #6097, #4189, #265, #6031, #8952, #4121, #10980, #7163, #8064, #11933, #388, #11040, #12412, #8481, #2830, #5754, #12473, #10622, #10500, #3710, #8420, #9625, #11459, #9563, #11519, #2766, #6695, #10563, #1686, #3775, #8603, #6570, #3590, #1935, #6628, #933, #12535, #12290, #10435, #10373, #3651, #5568, #7653, #740, #7529, #1811, #7593, #8545, #12352, #7719 ),
 ( #11396, #863, #9438, #1746, #4800, #4545, #1873, #2705, #5697, #5627, #2894, #4733, #9501, #4607, #8665, #804, #3843, #11586, #5815, #6757, #9688, #7465, #11339, #6509, #2644, #4674, #9545, #1911, #11563, #3882, #1045, #20, #8644, #2997, #910, #10416, #5859, #7756, #12516, #5674, #2808, #6608, #781, #11628, #83, #4779, #5796, #6799, #4906, #8765, #2872, #5734, #843, #10665, #1975, #9666, #7823, #3820, #6733, #1730, #9728, #976, #5609, #4650, #8520, #3691, #7570, #11438, #10479, #4711, #3755, #11500, #6672, #10542, #1852, #2300, #10727, #214, #149, #5980, #4006, #9980, #3061, #9854, #4138, #9918, #10861, #2103, #10045, #2171, #1289, #1169, #12006, #5162, #3121, #1356, #5222, #7949, #5032, #3189, #11752, #4071, #8078, #6864, #9029, #6044, #1227, #5097, #9093, #8962, #8011, #11884, #7050, #10928, #7116, #2242, #4263, #341, #3250, #4204, #11945, #400, #1101, #8140, #2040, #5920, #9790, #4967, #8830, #10221, #5345, #6295, #11113, #11175, #3371, #10336, #5535, #1534, #4383, #7428, #9216, #3492, #644, #10276, #9400, #11231, #7363, #5475, #3554, #11298, #2361, #6353, #6231, #7176, #4507, #2418, #8260, #461, #10166, #10104, #2604, #1654, #9341, #8200, #8383, #2478, #12251, #522, #9278, #703, #8325, #5284, #4571, #6413, #4323, #12130, #3438, #1472, #7300, #6474, #1594, #11053, #5407, #9155, #582, #8443, #3308, #12070, #7240, #4448, #4694, #10400, #11610, #10585, #10521, #10648, #5593, #3736, #12438, #6653, #6781, #959, #824, #2791, #9526, #7490, #3802, #8567, #9464, #1961, #5841, #12376, #6590, #4633, #762, #7617, #10459, #1834, #11480, #3612, #9712, #1027, #8692, #2854, #8503, #4827, #11361, #2, #9651, #3676, #4760, #2669, #8627, #4888, #1896, #12313, #7742, #6532, #2732, #11545, #1711, #7554, #7681, #5653, #6717, #11424, #5717, #12497, #2918, #1769, #9584, #890, #5778, #3866, #11866, #10911, #10712, #6849, #6155, #5081, #3046, #11796, #10977, #2983, #1215, #9839, #8949, #10030, #9012, #262, #8749, #7805, #8061, #5014, #5146, #10773, #7869, #132, #8879, #4118, #2285, #2156, #4053, #65, #9966, #3103, #7996, #3173, #6973, #7036, #2226, #5904, #6094, #1273, #2087, #11677, #1338, #10842, #323, #4186, #3930 ) ),
 .UNSPECIFIED., .F., .F., .F. ) 
 B_SPLINE_SURFACE_WITH_KNOTS ( ( 2, 2 ),
 ( 3, 2, 2, 2, 2, 2, 2, 2, 2, 2, 2, 2, 2, 2, 2, 2, 2, 2, 2, 2, 2, 2, 2, 2, 2, 2, 2, 2, 2, 2, 2, 2, 2, 2, 2, 2, 2, 2, 2, 2, 2, 2, 2, 2, 2, 2, 2, 2, 2, 2, 2, 2, 2, 2, 2, 2, 2, 2, 2, 2, 2, 2, 2, 2, 2, 2, 2, 2, 2, 2, 2, 2, 2, 2, 2, 2, 2, 2, 2, 2, 2, 2, 2, 2, 2, 2, 2, 2, 2, 2, 2, 2, 2, 2, 2, 2, 2, 2, 2, 2, 2, 2, 2, 2, 2, 2, 2, 2, 2, 2, 2, 2, 2, 2, 2, 2, 2, 2, 2, 2, 2, 2, 2, 2, 2, 2, 2, 2, 2, 2, 2, 2, 2, 2, 2, 2, 2, 2, 2, 2, 2, 2, 2, 2, 2, 2, 2, 2, 2, 2, 3 ),
 ( 0.000000000000000000, 1.000000000000000000 ),
 ( 0.000000000000000000, 0.006666666666666667095, 0.01333333333333333419, 0.02000000000000000042, 0.02666666666666666838, 0.03333333333333333287, 0.04000000000000000083, 0.04666666666666666879, 0.05333333333333333676, 0.05999999999999999778, 0.06666666666666666574, 0.07333333333333333370, 0.08000000000000000167, 0.08666666666666666963, 0.09333333333333333759, 0.1000000000000000056, 0.1066666666666666735, 0.1133333333333333276, 0.1199999999999999956, 0.1266666666666666774, 0.1333333333333333315, 0.1400000000000000133, 0.1466666666666666674, 0.1533333333333333215, 0.1600000000000000033, 0.1666666666666666574, 0.1733333333333333393, 0.1799999999999999933, 0.1866666666666666752, 0.1933333333333333293, 0.2000000000000000111, 0.2066666666666666652, 0.2133333333333333470, 0.2200000000000000011, 0.2266666666666666552, 0.2333333333333333370, 0.2399999999999999911, 0.2466666666666666730, 0.2533333333333333548, 0.2600000000000000089, 0.2666666666666666630, 0.2733333333333333171, 0.2800000000000000266, 0.2866666666666666807, 0.2933333333333333348, 0.2999999999999999889, 0.3066666666666666430, 0.3133333333333333526, 0.3200000000000000067, 0.3266666666666666607, 0.3333333333333333148, 0.3400000000000000244, 0.3466666666666666785, 0.3533333333333333326, 0.3599999999999999867, 0.3666666666666666408, 0.3733333333333333504, 0.3800000000000000044, 0.3866666666666666585, 0.3933333333333333126, 0.4000000000000000222, 0.4066666666666666763, 0.4133333333333333304, 0.4199999999999999845, 0.4266666666666666941, 0.4333333333333333481, 0.4400000000000000022, 0.4466666666666666563, 0.4533333333333333104, 0.4600000000000000200, 0.4666666666666666741, 0.4733333333333333282, 0.4799999999999999822, 0.4866666666666666918, 0.4933333333333333459, 0.5000000000000000000, 0.5066666666666667096, 0.5133333333333333082, 0.5200000000000000178, 0.5266666666666666163, 0.5333333333333333259, 0.5400000000000000355, 0.5466666666666666341, 0.5533333333333333437, 0.5600000000000000533, 0.5666666666666666519, 0.5733333333333333615, 0.5799999999999999600, 0.5866666666666666696, 0.5933333333333333792, 0.5999999999999999778, 0.6066666666666666874, 0.6133333333333332860, 0.6199999999999999956, 0.6266666666666667052, 0.6333333333333333037, 0.6400000000000000133, 0.6466666666666666119, 0.6533333333333333215, 0.6600000000000000311, 0.6666666666666666297, 0.6733333333333333393, 0.6800000000000000488, 0.6866666666666666474, 0.6933333333333333570, 0.6999999999999999556, 0.7066666666666666652, 0.7133333333333333748, 0.7199999999999999734, 0.7266666666666666829, 0.7333333333333332815, 0.7399999999999999911, 0.7466666666666667007, 0.7533333333333332993, 0.7600000000000000089, 0.7666666666666667185, 0.7733333333333333171, 0.7800000000000000266, 0.7866666666666666252, 0.7933333333333333348, 0.8000000000000000444, 0.8066666666666666430, 0.8133333333333333526, 0.8199999999999999512, 0.8266666666666666607, 0.8333333333333333703, 0.8399999999999999689, 0.8466666666666666785, 0.8533333333333333881, 0.8599999999999999867, 0.8666666666666666963, 0.8733333333333332948, 0.8800000000000000044, 0.8866666666666667140, 0.8933333333333333126, 0.9000000000000000222, 0.9066666666666666208, 0.9133333333333333304, 0.9200000000000000400, 0.9266666666666666385, 0.9333333333333333481, 0.9399999999999999467, 0.9466666666666666563, 0.9533333333333333659, 0.9599999999999999645, 0.9666666666666666741, 0.9733333333333333837, 0.9799999999999999822, 0.9866666666666666918, 0.9933333333333332904, 1.000000000000000000 ),
 .UNSPECIFIED. ) 
 GEOMETRIC_REPRESENTATION_ITEM ( )  RATIONAL_B_SPLINE_SURFACE ( (
 ( 1.000000000000000000, 0.9510565162951535312, 1.000000000000000000, 0.9510565162951535312, 1.000000000000000000, 0.9510565162951535312, 1.000000000000000000, 0.9510565162951535312, 1.000000000000000000, 0.9510565162951535312, 1.000000000000000000, 0.9510565162951535312, 1.000000000000000000, 0.9510565162951535312, 1.000000000000000000, 0.9510565162951535312, 1.000000000000000000, 0.9510565162951535312, 1.000000000000000000, 0.9510565162951535312, 1.000000000000000000, 0.9510565162951535312, 1.000000000000000000, 0.9510565162951535312, 1.000000000000000000, 0.9510565162951535312, 1.000000000000000000, 0.9510565162951535312, 1.000000000000000000, 0.9510565162951535312, 1.000000000000000000, 0.9510565162951535312, 1.000000000000000000, 0.9510565162951535312, 1.000000000000000000, 0.9510565162951535312, 1.000000000000000000, 0.9510565162951535312, 1.000000000000000000, 0.9510565162951535312, 1.000000000000000000, 0.9510565162951535312, 1.000000000000000000, 0.9510565162951535312, 1.000000000000000000, 0.9510565162951535312, 1.000000000000000000, 0.9510565162951535312, 1.000000000000000000, 0.9510565162951535312, 1.000000000000000000, 0.9510565162951535312, 1.000000000000000000, 0.9510565162951535312, 1.000000000000000000, 0.9510565162951535312, 1.000000000000000000, 0.9510565162951535312, 1.000000000000000000, 0.9510565162951535312, 1.000000000000000000, 0.9510565162951535312, 1.000000000000000000, 0.9510565162951535312, 1.000000000000000000, 0.9510565162951535312, 1.000000000000000000, 0.9510565162951535312, 1.000000000000000000, 0.9510565162951535312, 1.000000000000000000, 0.9510565162951535312, 1.000000000000000000, 0.9510565162951535312, 1.000000000000000000, 0.9510565162951535312, 1.000000000000000000, 0.9510565162951535312, 1.000000000000000000, 0.9510565162951535312, 1.000000000000000000, 0.9510565162951535312, 1.000000000000000000, 0.9510565162951535312, 1.000000000000000000, 0.9510565162951535312, 1.000000000000000000, 0.9510565162951535312, 1.000000000000000000, 0.9510565162951535312, 1.000000000000000000, 0.9510565162951535312, 1.000000000000000000, 0.9510565162951535312, 1.000000000000000000, 0.9510565162951535312, 1.000000000000000000, 0.9510565162951535312, 1.000000000000000000, 0.9510565162951535312, 1.000000000000000000, 0.9510565162951535312, 1.000000000000000000, 0.9510565162951535312, 1.000000000000000000, 0.9510565162951535312, 1.000000000000000000, 0.9510565162951535312, 1.000000000000000000, 0.9510565162951535312, 1.000000000000000000, 0.9510565162951535312, 1.000000000000000000, 0.9510565162951535312, 1.000000000000000000, 0.9510565162951535312, 1.000000000000000000, 0.9510565162951535312, 1.000000000000000000, 0.9510565162951535312, 1.000000000000000000, 0.9510565162951535312, 1.000000000000000000, 0.9510565162951535312, 1.000000000000000000, 0.9510565162951535312, 1.000000000000000000, 0.9510565162951535312, 1.000000000000000000, 0.9510565162951535312, 1.000000000000000000, 0.9510565162951535312, 1.000000000000000000, 0.9510565162951535312, 1.000000000000000000, 0.9510565162951535312, 1.000000000000000000, 0.9510565162951535312, 1.000000000000000000, 0.9510565162951535312, 1.000000000000000000, 0.9510565162951535312, 1.000000000000000000, 0.9510565162951535312, 1.000000000000000000, 0.9510565162951535312, 1.000000000000000000, 0.9510565162951535312, 1.000000000000000000, 0.9510565162951535312, 1.000000000000000000, 0.9510565162951535312, 1.000000000000000000, 0.9510565162951535312, 1.000000000000000000, 0.9510565162951535312, 1.000000000000000000, 0.9510565162951535312, 1.000000000000000000, 0.9510565162951535312, 1.000000000000000000, 0.9510565162951535312, 1.000000000000000000, 0.9510565162951535312, 1.000000000000000000, 0.9510565162951535312, 1.000000000000000000, 0.9510565162951535312, 1.000000000000000000, 0.9510565162951535312, 1.000000000000000000, 0.9510565162951535312, 1.000000000000000000, 0.9510565162951535312, 1.000000000000000000, 0.9510565162951535312, 1.000000000000000000, 0.9510565162951535312, 1.000000000000000000, 0.9510565162951535312, 1.000000000000000000, 0.9510565162951535312, 1.000000000000000000, 0.9510565162951535312, 1.000000000000000000, 0.9510565162951535312, 1.000000000000000000, 0.9510565162951535312, 1.000000000000000000, 0.9510565162951535312, 1.000000000000000000, 0.9510565162951535312, 1.000000000000000000, 0.9510565162951535312, 1.000000000000000000, 0.9510565162951535312, 1.000000000000000000, 0.9510565162951535312, 1.000000000000000000, 0.9510565162951535312, 1.000000000000000000, 0.9510565162951535312, 1.000000000000000000, 0.9510565162951535312, 1.000000000000000000, 0.9510565162951535312, 1.000000000000000000, 0.9510565162951535312, 1.000000000000000000, 0.9510565162951535312, 1.000000000000000000, 0.9510565162951535312, 1.000000000000000000, 0.9510565162951535312, 1.000000000000000000, 0.9510565162951535312, 1.000000000000000000, 0.9510565162951535312, 1.000000000000000000, 0.9510565162951535312, 1.000000000000000000, 0.9510565162951535312, 1.000000000000000000, 0.9510565162951535312, 1.000000000000000000, 0.9510565162951535312, 1.000000000000000000, 0.9510565162951535312, 1.000000000000000000, 0.9510565162951535312, 1.000000000000000000, 0.9510565162951535312, 1.000000000000000000, 0.9510565162951535312, 1.000000000000000000, 0.9510565162951535312, 1.000000000000000000, 0.9510565162951535312, 1.000000000000000000, 0.9510565162951535312, 1.000000000000000000, 0.9510565162951535312, 1.000000000000000000, 0.9510565162951535312, 1.000000000000000000, 0.9510565162951535312, 1.000000000000000000, 0.9510565162951535312, 1.000000000000000000, 0.9510565162951535312, 1.000000000000000000, 0.9510565162951535312, 1.000000000000000000, 0.9510565162951535312, 1.000000000000000000, 0.9510565162951535312, 1.000000000000000000, 0.9510565162951535312, 1.000000000000000000, 0.9510565162951535312, 1.000000000000000000, 0.9510565162951535312, 1.000000000000000000, 0.9510565162951535312, 1.000000000000000000, 0.9510565162951535312, 1.000000000000000000, 0.9510565162951535312, 1.000000000000000000, 0.9510565162951535312, 1.000000000000000000, 0.9510565162951535312, 1.000000000000000000, 0.9510565162951535312, 1.000000000000000000, 0.9510565162951535312, 1.000000000000000000, 0.9510565162951535312, 1.000000000000000000, 0.9510565162951535312, 1.000000000000000000, 0.9510565162951535312, 1.000000000000000000, 0.9510565162951535312, 1.000000000000000000, 0.9510565162951535312, 1.000000000000000000, 0.9510565162951535312, 1.000000000000000000, 0.9510565162951535312, 1.000000000000000000, 0.9510565162951535312, 1.000000000000000000, 0.9510565162951535312, 1.000000000000000000, 0.9510565162951535312, 1.000000000000000000, 0.9510565162951535312, 1.000000000000000000, 0.9510565162951535312, 1.000000000000000000),
 ( 1.000000000000000000, 0.9510565162951535312, 1.000000000000000000, 0.9510565162951535312, 1.000000000000000000, 0.9510565162951535312, 1.000000000000000000, 0.9510565162951535312, 1.000000000000000000, 0.9510565162951535312, 1.000000000000000000, 0.9510565162951535312, 1.000000000000000000, 0.9510565162951535312, 1.000000000000000000, 0.9510565162951535312, 1.000000000000000000, 0.9510565162951535312, 1.000000000000000000, 0.9510565162951535312, 1.000000000000000000, 0.9510565162951535312, 1.000000000000000000, 0.9510565162951535312, 1.000000000000000000, 0.9510565162951535312, 1.000000000000000000, 0.9510565162951535312, 1.000000000000000000, 0.9510565162951535312, 1.000000000000000000, 0.9510565162951535312, 1.000000000000000000, 0.9510565162951535312, 1.000000000000000000, 0.9510565162951535312, 1.000000000000000000, 0.9510565162951535312, 1.000000000000000000, 0.9510565162951535312, 1.000000000000000000, 0.9510565162951535312, 1.000000000000000000, 0.9510565162951535312, 1.000000000000000000, 0.9510565162951535312, 1.000000000000000000, 0.9510565162951535312, 1.000000000000000000, 0.9510565162951535312, 1.000000000000000000, 0.9510565162951535312, 1.000000000000000000, 0.9510565162951535312, 1.000000000000000000, 0.9510565162951535312, 1.000000000000000000, 0.9510565162951535312, 1.000000000000000000, 0.9510565162951535312, 1.000000000000000000, 0.9510565162951535312, 1.000000000000000000, 0.9510565162951535312, 1.000000000000000000, 0.9510565162951535312, 1.000000000000000000, 0.9510565162951535312, 1.000000000000000000, 0.9510565162951535312, 1.000000000000000000, 0.9510565162951535312, 1.000000000000000000, 0.9510565162951535312, 1.000000000000000000, 0.9510565162951535312, 1.000000000000000000, 0.9510565162951535312, 1.000000000000000000, 0.9510565162951535312, 1.000000000000000000, 0.9510565162951535312, 1.000000000000000000, 0.9510565162951535312, 1.000000000000000000, 0.9510565162951535312, 1.000000000000000000, 0.9510565162951535312, 1.000000000000000000, 0.9510565162951535312, 1.000000000000000000, 0.9510565162951535312, 1.000000000000000000, 0.9510565162951535312, 1.000000000000000000, 0.9510565162951535312, 1.000000000000000000, 0.9510565162951535312, 1.000000000000000000, 0.9510565162951535312, 1.000000000000000000, 0.9510565162951535312, 1.000000000000000000, 0.9510565162951535312, 1.000000000000000000, 0.9510565162951535312, 1.000000000000000000, 0.9510565162951535312, 1.000000000000000000, 0.9510565162951535312, 1.000000000000000000, 0.9510565162951535312, 1.000000000000000000, 0.9510565162951535312, 1.000000000000000000, 0.9510565162951535312, 1.000000000000000000, 0.9510565162951535312, 1.000000000000000000, 0.9510565162951535312, 1.000000000000000000, 0.9510565162951535312, 1.000000000000000000, 0.9510565162951535312, 1.000000000000000000, 0.9510565162951535312, 1.000000000000000000, 0.9510565162951535312, 1.000000000000000000, 0.9510565162951535312, 1.000000000000000000, 0.9510565162951535312, 1.000000000000000000, 0.9510565162951535312, 1.000000000000000000, 0.9510565162951535312, 1.000000000000000000, 0.9510565162951535312, 1.000000000000000000, 0.9510565162951535312, 1.000000000000000000, 0.9510565162951535312, 1.000000000000000000, 0.9510565162951535312, 1.000000000000000000, 0.9510565162951535312, 1.000000000000000000, 0.9510565162951535312, 1.000000000000000000, 0.9510565162951535312, 1.000000000000000000, 0.9510565162951535312, 1.000000000000000000, 0.9510565162951535312, 1.000000000000000000, 0.9510565162951535312, 1.000000000000000000, 0.9510565162951535312, 1.000000000000000000, 0.9510565162951535312, 1.000000000000000000, 0.9510565162951535312, 1.000000000000000000, 0.9510565162951535312, 1.000000000000000000, 0.9510565162951535312, 1.000000000000000000, 0.9510565162951535312, 1.000000000000000000, 0.9510565162951535312, 1.000000000000000000, 0.9510565162951535312, 1.000000000000000000, 0.9510565162951535312, 1.000000000000000000, 0.9510565162951535312, 1.000000000000000000, 0.9510565162951535312, 1.000000000000000000, 0.9510565162951535312, 1.000000000000000000, 0.9510565162951535312, 1.000000000000000000, 0.9510565162951535312, 1.000000000000000000, 0.9510565162951535312, 1.000000000000000000, 0.9510565162951535312, 1.000000000000000000, 0.9510565162951535312, 1.000000000000000000, 0.9510565162951535312, 1.000000000000000000, 0.9510565162951535312, 1.000000000000000000, 0.9510565162951535312, 1.000000000000000000, 0.9510565162951535312, 1.000000000000000000, 0.9510565162951535312, 1.000000000000000000, 0.9510565162951535312, 1.000000000000000000, 0.9510565162951535312, 1.000000000000000000, 0.9510565162951535312, 1.000000000000000000, 0.9510565162951535312, 1.000000000000000000, 0.9510565162951535312, 1.000000000000000000, 0.9510565162951535312, 1.000000000000000000, 0.9510565162951535312, 1.000000000000000000, 0.9510565162951535312, 1.000000000000000000, 0.9510565162951535312, 1.000000000000000000, 0.9510565162951535312, 1.000000000000000000, 0.9510565162951535312, 1.000000000000000000, 0.9510565162951535312, 1.000000000000000000, 0.9510565162951535312, 1.000000000000000000, 0.9510565162951535312, 1.000000000000000000, 0.9510565162951535312, 1.000000000000000000, 0.9510565162951535312, 1.000000000000000000, 0.9510565162951535312, 1.000000000000000000, 0.9510565162951535312, 1.000000000000000000, 0.9510565162951535312, 1.000000000000000000, 0.9510565162951535312, 1.000000000000000000, 0.9510565162951535312, 1.000000000000000000, 0.9510565162951535312, 1.000000000000000000, 0.9510565162951535312, 1.000000000000000000, 0.9510565162951535312, 1.000000000000000000, 0.9510565162951535312, 1.000000000000000000, 0.9510565162951535312, 1.000000000000000000, 0.9510565162951535312, 1.000000000000000000, 0.9510565162951535312, 1.000000000000000000, 0.9510565162951535312, 1.000000000000000000, 0.9510565162951535312, 1.000000000000000000, 0.9510565162951535312, 1.000000000000000000, 0.9510565162951535312, 1.000000000000000000, 0.9510565162951535312, 1.000000000000000000, 0.9510565162951535312, 1.000000000000000000, 0.9510565162951535312, 1.000000000000000000, 0.9510565162951535312, 1.000000000000000000, 0.9510565162951535312, 1.000000000000000000, 0.9510565162951535312, 1.000000000000000000, 0.9510565162951535312, 1.000000000000000000, 0.9510565162951535312, 1.000000000000000000, 0.9510565162951535312, 1.000000000000000000, 0.9510565162951535312, 1.000000000000000000, 0.9510565162951535312, 1.000000000000000000, 0.9510565162951535312, 1.000000000000000000, 0.9510565162951535312, 1.000000000000000000, 0.9510565162951535312, 1.000000000000000000, 0.9510565162951535312, 1.000000000000000000, 0.9510565162951535312, 1.000000000000000000, 0.9510565162951535312, 1.000000000000000000, 0.9510565162951535312, 1.000000000000000000) ) ) 
 REPRESENTATION_ITEM ( '' )  SURFACE ( )  );
#10218 = CARTESIAN_POINT ( 'NONE',  ( 34.67500000054622689, 15.71886984736413773, 84.90069139318163138 ) ) ;
#10219 = FACE_OUTER_BOUND ( 'NONE', #11732, .T. ) ;
#10220 = CARTESIAN_POINT ( 'NONE',  ( 45.47500000054623115, 26.19570976099943849, 95.29460816699764791 ) ) ;
#10221 = CARTESIAN_POINT ( 'NONE',  ( 36.97500000054623115, 22.36655054427230382, 83.50966788445364841 ) ) ;
#10222 = CARTESIAN_POINT ( 'NONE',  ( 33.49999999999998579, 27.88596668178699645, 90.79316153445363113 ) ) ;
#10223 = CARTESIAN_POINT ( 'NONE',  ( -6.116604691219384549, 27.93765947712327247, 20.09721008222173211 ) ) ;
#10224 = CARTESIAN_POINT ( 'NONE',  ( 41.47500000054623115, 26.19570976099943493, 95.29460816699764791 ) ) ;
#10225 = EDGE_LOOP ( 'NONE', ( #807, #4376, #4715, #8102 ) ) ;
#10226 = AXIS2_PLACEMENT_3D ( 'NONE', #9699, #8494, #8680 ) ;
#10227 = CARTESIAN_POINT ( 'NONE',  ( 26.25000000109246656, 12.86707612778636012, 88.47553407664152303 ) ) ;
#10228 = DIRECTION ( 'NONE',  ( 0.000000000000000000, 0.000000000000000000, -1.000000000000000000 ) ) ;
#10229 = VERTEX_POINT ( 'NONE', #5065 ) ;
#10230 =( REPRESENTATION_RELATIONSHIP ('NONE','NONE', #4262, #10013 ) REPRESENTATION_RELATIONSHIP_WITH_TRANSFORMATION ( #317 )SHAPE_REPRESENTATION_RELATIONSHIP( ) );
#10231 = DIRECTION ( 'NONE',  ( 1.000000000000000000, 0.000000000000000000, 0.000000000000000000 ) ) ;
#10232 = ORIENTED_EDGE ( 'NONE', *, *, #12017, .F. ) ;
#10233 = FACE_OUTER_BOUND ( 'NONE', #2303, .T. ) ;
#10234 = CARTESIAN_POINT ( 'NONE',  ( 3.429011037612589670E-15, 0.000000000000000000, 28.00000000000000355 ) ) ;
#10235 = CARTESIAN_POINT ( 'NONE',  ( 36.35000000109246798, 13.62011893735970958, 86.15790661882942914 ) ) ;
#10236 = CARTESIAN_POINT ( 'NONE',  ( 32.25000000109245946, 12.86707612778636012, 88.47553407664152303 ) ) ;
#10237 = EDGE_CURVE ( 'NONE', #4148, #8970, #151, .T. ) ;
#10238 = CARTESIAN_POINT ( 'NONE',  ( 25.47500000054622760, 26.19570976099943493, 95.29460816699764791 ) ) ;
#10239 = CARTESIAN_POINT ( 'NONE',  ( 27.07500000054622546, 24.28113015263587471, 84.90069139318163138 ) ) ;
#10240 = CARTESIAN_POINT ( 'NONE',  ( 8.125441273627673766, 25.83810069393247488, 26.79577025665707879 ) ) ;
#10241 = CARTESIAN_POINT ( 'NONE',  ( 20.27158385259951956, 22.00000000000000000, 170.0000119999999697 ) ) ;
#10242 = ORIENTED_EDGE ( 'NONE', *, *, #11183, .F. ) ;
#10243 = VECTOR ( 'NONE', #11148, 1000.000000000000000 ) ;
#10244 = CARTESIAN_POINT ( 'NONE',  ( 42.85000000109246798, 24.40838939219355197, 84.72553407664153724 ) ) ;
#10245 = EDGE_LOOP ( 'NONE', ( #3485, #3616, #1250, #8021 ) ) ;
#10246 = LINE ( 'NONE', #5310, #11333 ) ;
#10247 = VERTEX_POINT ( 'NONE', #8799 ) ;
#10248 = CARTESIAN_POINT ( 'NONE',  ( 4.741197079555949934, 51.62084573238831098, 20.45818942849235000 ) ) ;
#10249 = DIRECTION ( 'NONE',  ( -1.000000000000000000, -0.000000000000000000, -0.000000000000000000 ) ) ;
#10250 = CARTESIAN_POINT ( 'NONE',  ( 20.27500000054623186, 12.34168156654572535, 90.79316153445363113 ) ) ;
#10251 = DIRECTION ( 'NONE',  ( 0.000000000000000000, 0.4999999999999989453, -0.8660254037844391517 ) ) ;
#10252 = CARTESIAN_POINT ( 'NONE',  ( -1.332521848768800865, 10.08356887257211199, 20.96031352669567838 ) ) ;
#10253 = ADVANCED_FACE ( 'NONE', ( #7916 ), #4169, .F. ) ;
#10254 = CARTESIAN_POINT ( 'NONE',  ( 0.000000000000000000, 20.00000000000000355, -66.99999999999998579 ) ) ;
#10255 = PLANE ( 'NONE',  #2349 ) ;
#10256 = CARTESIAN_POINT ( 'NONE',  ( -2.508190414677843982, 54.33763061856527088, 24.87535316732256163 ) ) ;
#10257 = EDGE_LOOP ( 'NONE', ( #10004, #8636, #3496, #10673, #71, #11167 ) ) ;
#10258 = ADVANCED_FACE ( 'NONE', ( #3154 ), #11781, .F. ) ;
#10259 = CARTESIAN_POINT ( 'NONE',  ( 49.99999999999998579, 20.00000000000000355, 90.79316153445363113 ) ) ;
#10260 = CARTESIAN_POINT ( 'NONE',  ( 47.65000000109246514, 20.00000000000000355, 98.29316153445363113 ) ) ;
#10261 = CARTESIAN_POINT ( 'NONE',  ( 39.57500000054623257, 26.19570976099943493, 95.29460816699764791 ) ) ;
#10262 = AXIS2_PLACEMENT_3D ( 'NONE', #19, #4710, #82 ) ;
#10263 = CARTESIAN_POINT ( 'NONE',  ( 25.17500000054623044, 26.92701409722686634, 88.54243821818162985 ) ) ;
#10264 = CARTESIAN_POINT ( 'NONE',  ( 6.614374549531869540, 12.49999671209873497, 91.04913669327301307 ) ) ;
#10265 = CARTESIAN_POINT ( 'NONE',  ( 22.65000000109246514, 20.00000000000000355, 83.29316153445364534 ) ) ;
#10266 = CARTESIAN_POINT ( 'NONE',  ( -2.000000000000015543, 20.00000000000000355, 90.79316153445363113 ) ) ;
#10267 = CARTESIAN_POINT ( 'NONE',  ( 31.09999999999998721, 22.43689772174679575, 83.29316153445363113 ) ) ;
#10268 = ORIENTED_EDGE ( 'NONE', *, *, #9066, .T. ) ;
#10269 = CARTESIAN_POINT ( 'NONE',  ( 0.000000000000000000, 20.00000000000000355, 109.9999999999999858 ) ) ;
#10270 = VERTEX_POINT ( 'NONE', #5824 ) ;
#10271 = FACE_OUTER_BOUND ( 'NONE', #2531, .T. ) ;
#10272 = CARTESIAN_POINT ( 'NONE',  ( 23.99999999999998579, 76.99999999999998579, 146.8533255156882547 ) ) ;
#10273 = CARTESIAN_POINT ( 'NONE',  ( 31.67500000054622333, 24.28113015263587116, 96.68563167572563088 ) ) ;
#10274 = CARTESIAN_POINT ( 'NONE',  ( 27.65000000109246514, 20.00000000000000355, 98.29316153445363113 ) ) ;
#10275 = CARTESIAN_POINT ( 'NONE',  ( 47.37500000054622973, 26.92701409722686634, 93.04388485072563242 ) ) ;
#10276 = CARTESIAN_POINT ( 'NONE',  ( 35.57500000054623257, 26.19570976099943493, 95.29460816699764791 ) ) ;
#10277 = CARTESIAN_POINT ( 'NONE',  ( 37.59999999999998721, 27.13292387221364876, 93.11078899226573924 ) ) ;
#10278 = CARTESIAN_POINT ( 'NONE',  ( 5.000000000000000000, 2.342598717236900718, -4.057500000000001883 ) ) ;
#10279 = EDGE_CURVE ( 'NONE', #707, #10641, #2149, .T. ) ;
#10280 = CARTESIAN_POINT ( 'NONE',  ( 37.47500000054623825, 26.19570976099943493, 95.29460816699764791 ) ) ;
#10281 = ORIENTED_EDGE ( 'NONE', *, *, #6802, .F. ) ;
#10282 = CARTESIAN_POINT ( 'NONE',  ( 21.15000000109246514, 27.88596668178699645, 90.79316153445363113 ) ) ;
#10283 = CARTESIAN_POINT ( 'NONE',  ( -50.00000000000001421, 55.00000000000000000, 166.8533255156881694 ) ) ;
#10284 = EDGE_LOOP ( 'NONE', ( #7040, #7873, #9674 ) ) ;
#10285 = DIRECTION ( 'NONE',  ( 0.000000000000000000, 0.000000000000000000, 1.000000000000000000 ) ) ;
#10286 = VERTEX_POINT ( 'NONE', #9886 ) ;
#10287 =( BOUNDED_CURVE ( )  B_SPLINE_CURVE ( 2, ( #11497, #10352, #12452, #4709, #6548, #11314, #6730, #6606, #5732, #2870, #4523 ),
 .UNSPECIFIED., .F., .F. ) 
 B_SPLINE_CURVE_WITH_KNOTS ( ( 3, 2, 2, 2, 2, 3 ),
 ( 0.9666666666666666741, 0.9733333333333333837, 0.9799999999999999822, 0.9866666666666666918, 0.9933333333333332904, 1.000000000000000000 ),
 .UNSPECIFIED. ) 
 CURVE ( )  GEOMETRIC_REPRESENTATION_ITEM ( )  RATIONAL_B_SPLINE_CURVE ( ( 1.000000000000000000, 0.9510565162951535312, 1.000000000000000000, 0.9510565162951535312, 1.000000000000000000, 0.9510565162951535312, 1.000000000000000000, 0.9510565162951535312, 1.000000000000000000, 0.9510565162951535312, 1.000000000000000000 ) ) 
 REPRESENTATION_ITEM ( '' )  );
#10288 = VECTOR ( 'NONE', #9112, 1000.000000000000000 ) ;
#10289 = DIRECTION ( 'NONE',  ( 0.000000000000000000, 0.5000000000000011102, 0.8660254037844379305 ) ) ;
#10290 = CARTESIAN_POINT ( 'NONE',  ( 4.999999999999999112, 22.00000000000000000, 169.9999999999999716 ) ) ;
#10291 = CARTESIAN_POINT ( 'NONE',  ( 25.89999999999998792, 22.43689772174679575, 98.29316153445363113 ) ) ;
#10292 = CARTESIAN_POINT ( 'NONE',  ( 24.17500000054622689, 13.07298590277314254, 93.04388485072563242 ) ) ;
#10293 = CARTESIAN_POINT ( 'NONE',  ( 25.97500000054622049, 17.63344945572769973, 98.07665518445361386 ) ) ;
#10294 = DIRECTION ( 'NONE',  ( 0.000000000000000000, 0.000000000000000000, 1.000000000000000000 ) ) ;
#10295 = CARTESIAN_POINT ( 'NONE',  ( -2.000000000000015543, 20.00000000000000355, 83.29316153445364534 ) ) ;
#10296 = VECTOR ( 'NONE', #2905, 1000.000000000000000 ) ;
#10297 = VERTEX_POINT ( 'NONE', #5128 ) ;
#10298 = CARTESIAN_POINT ( 'NONE',  ( 36.35000000109246798, 13.62011893735971135, 86.15790661882942914 ) ) ;
#10299 =( NAMED_UNIT ( * ) PLANE_ANGLE_UNIT ( ) SI_UNIT ( $, .RADIAN. ) );
#10300 = VERTEX_POINT ( 'NONE', #11722 ) ;
#10301 = LINE ( 'NONE', #3578, #8292 ) ;
#10302 = EDGE_CURVE ( 'NONE', #10109, #11432, #6080, .T. ) ;
#10303 = ORIENTED_EDGE ( 'NONE', *, *, #2491, .F. ) ;
#10304 = CARTESIAN_POINT ( 'NONE',  ( 6.000000000000000000, 5.839897972853064445, -8.673617379884035472E-15 ) ) ;
#10305 = CARTESIAN_POINT ( 'NONE',  ( 5.307486386703490489, 11.51851869311760090, -24.43167369944409018 ) ) ;
#10306 = EDGE_CURVE ( 'NONE', #9039, #7786, #6012, .T. ) ;
#10307 = DIRECTION ( 'NONE',  ( -1.000000000000000000, -0.000000000000000000, -0.000000000000000000 ) ) ;
#10308 = CARTESIAN_POINT ( 'NONE',  ( 4.999999999999999112, 0.000000000000000000, 169.9999999999999716 ) ) ;
#10309 = CARTESIAN_POINT ( 'NONE',  ( 42.09999999999997300, 17.56310227825320425, 98.29316153445363113 ) ) ;
#10310 = FACE_OUTER_BOUND ( 'NONE', #2180, .T. ) ;
#10311 = CARTESIAN_POINT ( 'NONE',  ( 27.77500000054622831, 20.00000000000000355, 98.07665518445361386 ) ) ;
#10312 = CARTESIAN_POINT ( 'NONE',  ( 9.465308527890080370, 23.24274166418333110, 23.13911695433847981 ) ) ;
#10313 = CARTESIAN_POINT ( 'NONE',  ( 46.65000000109246514, 20.00000000000000355, 83.29316153445364534 ) ) ;
#10314 = EDGE_LOOP ( 'NONE', ( #3516, #158, #1296, #12520 ) ) ;
#10315 = AXIS2_PLACEMENT_3D ( 'NONE', #8593, #9676, #12463 ) ;
#10316 = CARTESIAN_POINT ( 'NONE',  ( 4.839779845606726916, 48.70264860999793655, 24.52714343409649089 ) ) ;
#10317 = EDGE_CURVE ( 'NONE', #10297, #4126, #3975, .T. ) ;
#10318 = CARTESIAN_POINT ( 'NONE',  ( 6.000000000000000000, 5.839897972853064445, -8.673617379884035472E-15 ) ) ;
#10319 = CARTESIAN_POINT ( 'NONE',  ( 37.77500000054623541, 20.00000000000000355, 98.07665518445361386 ) ) ;
#10320 = CARTESIAN_POINT ( 'NONE',  ( 38.87500000054622262, 20.00000000000000355, 83.50966788445364841 ) ) ;
#10321 = CARTESIAN_POINT ( 'NONE',  ( 29.17500000054623044, 26.92701409722686634, 88.54243821818162985 ) ) ;
#10322 = CARTESIAN_POINT ( 'NONE',  ( 6.732675160020738403, 12.60562763040432621, 89.51398028008233609 ) ) ;
#10323 = CARTESIAN_POINT ( 'NONE',  ( -9.983825383151277322, 20.65789756057008120, 22.91995855732452370 ) ) ;
#10324 = DIRECTION ( 'NONE',  ( 1.000000000000000000, -0.000000000000000000, -0.000000000000000000 ) ) ;
#10325 = DIRECTION ( 'NONE',  ( 1.000000000000000000, -0.000000000000000000, -0.000000000000000000 ) ) ;
#10326 = EDGE_CURVE ( 'NONE', #223, #11822, #11151, .T. ) ;
#10327 = EDGE_LOOP ( 'NONE', ( #7761, #7215, #544, #2976, #3278, #360, #11718, #7291, #3330, #11761, #239, #426, #6406, #4028, #6600, #11485 ) ) ;
#10328 = DIRECTION ( 'NONE',  ( 0.000000000000000000, 0.000000000000000000, 1.000000000000000000 ) ) ;
#10329 = VERTEX_POINT ( 'NONE', #306 ) ;
#10330 = VECTOR ( 'NONE', #2030, 1000.000000000000000 ) ;
#10331 = DIRECTION ( 'NONE',  ( -1.000000000000000000, 0.000000000000000000, -0.000000000000000000 ) ) ;
#10332 = APPLICATION_PROTOCOL_DEFINITION ( 'draft international standard', 'automotive_design', 1998, #2215 ) ;
#10333 = CARTESIAN_POINT ( 'NONE',  ( 35.17500000054621268, 26.19570976099943849, 86.29171490190961435 ) ) ;
#10334 = CARTESIAN_POINT ( 'NONE',  ( 26.95000000109246585, 26.37988106264029398, 86.15790661882942914 ) ) ;
#10335 = CARTESIAN_POINT ( 'NONE',  ( 46.17500000054623399, 13.07298590277314254, 93.04388485072563242 ) ) ;
#10336 = CARTESIAN_POINT ( 'NONE',  ( 36.37500000054623683, 12.34168156654572535, 90.79316153445363113 ) ) ;
#10337 = CARTESIAN_POINT ( 'NONE',  ( 30.19999999999998863, 15.59161060780645691, 96.86078899226572503 ) ) ;
#10338 = VECTOR ( 'NONE', #9393, 1000.000000000000000 ) ;
#10339 = CARTESIAN_POINT ( 'NONE',  ( 4.149575074854375600, 29.10425525072577102, 24.65509887497819008 ) ) ;
#10340 = CARTESIAN_POINT ( 'NONE',  ( 40.67500000054623399, 17.63344945572770328, 83.50966788445364841 ) ) ;
#10341 = EDGE_LOOP ( 'NONE', ( #10303, #8033, #3394 ) ) ;
#10342 = CARTESIAN_POINT ( 'NONE',  ( 49.57500000054623257, 24.28113015263587116, 96.68563167572563088 ) ) ;
#10343 = CARTESIAN_POINT ( 'NONE',  ( 27.85000000109246443, 15.59161060780645691, 96.86078899226572503 ) ) ;
#10344 = ORIENTED_EDGE ( 'NONE', *, *, #3730, .F. ) ;
#10345 = CARTESIAN_POINT ( 'NONE',  ( 7.924332520748174957, 13.89188147265340945, 19.44874353718065763 ) ) ;
#10346 = EDGE_LOOP ( 'NONE', ( #6677, #24 ) ) ;
#10347 = CARTESIAN_POINT ( 'NONE',  ( 9.658351069856484727, 22.61227114741398836, -23.05920763558311037 ) ) ;
#10348 = AXIS2_PLACEMENT_3D ( 'NONE', #1467, #9209, #516 ) ;
#10349 = CARTESIAN_POINT ( 'NONE',  ( 9.933941257241759359, 18.67913347266169666, 26.17891498049026211 ) ) ;
#10350 = DIRECTION ( 'NONE',  ( 0.000000000000000000, 0.000000000000000000, 1.000000000000000000 ) ) ;
#10351 = EDGE_CURVE ( 'NONE', #9812, #5818, #11848, .T. ) ;
#10352 = CARTESIAN_POINT ( 'NONE',  ( 20.89999999999999147, 17.56310227825320425, 83.29316153445363113 ) ) ;
#10353 = CARTESIAN_POINT ( 'NONE',  ( 24.47500000054623115, 13.80429023900056684, 86.29171490190961435 ) ) ;
#10354 = CARTESIAN_POINT ( 'NONE',  ( 21.87500000054622618, 20.00000000000000355, 98.07665518445361386 ) ) ;
#10355 = AXIS2_PLACEMENT_3D ( 'NONE', #10485, #12459, #10548 ) ;
#10356 = DIRECTION ( 'NONE',  ( 0.000000000000000000, -1.000000000000000000, 1.336710962791342904E-15 ) ) ;
#10357 = DIRECTION ( 'NONE',  ( 1.000000000000000000, -0.000000000000000000, -0.000000000000000000 ) ) ;
#10358 = ORIENTED_EDGE ( 'NONE', *, *, #8225, .F. ) ;
#10359 = CARTESIAN_POINT ( 'NONE',  ( 35.45000000109246940, 24.40838939219354842, 96.86078899226572503 ) ) ;
#10360 = CARTESIAN_POINT ( 'NONE',  ( 24.99999999999998579, 20.00000000000000355, 83.29316153445364534 ) ) ;
#10361 = ORIENTED_EDGE ( 'NONE', *, *, #7728, .T. ) ;
#10362 = CARTESIAN_POINT ( 'NONE',  ( 47.79999999999999005, 24.40838939219354842, 96.86078899226572503 ) ) ;
#10363 = ORIENTED_EDGE ( 'NONE', *, *, #7196, .F. ) ;
#10364 = CARTESIAN_POINT ( 'NONE',  ( -50.00000000000001421, 55.00000000000000000, 124.8533255156881694 ) ) ;
#10365 = CARTESIAN_POINT ( 'NONE',  ( 0.000000000000000000, 50.00000000000000000, -28.00000000000000711 ) ) ;
#10366 = EDGE_CURVE ( 'NONE', #12065, #801, #245, .T. ) ;
#10367 = CARTESIAN_POINT ( 'NONE',  ( -3.243418093453738216, 29.48203249043655561, 24.79625640031606082 ) ) ;
#10368 = EDGE_CURVE ( 'NONE', #7937, #3410, #355, .T. ) ;
#10369 = CARTESIAN_POINT ( 'NONE',  ( 1.500000000000001332, 0.000000000000000000, 0.000000000000000000 ) ) ;
#10370 = CARTESIAN_POINT ( 'NONE',  ( 2.571758291765529985E-15, 45.00000000000000711, 21.00000000000000000 ) ) ;
#10371 = LINE ( 'NONE', #11517, #7381 ) ;
#10372 = CARTESIAN_POINT ( 'NONE',  ( -4.446180375167638310, 11.03685037693071891, 27.64627648346033340 ) ) ;
#10373 = CARTESIAN_POINT ( 'NONE',  ( 20.77500000054622831, 20.00000000000000355, 83.50966788445364841 ) ) ;
#10374 = DIRECTION ( 'NONE',  ( 1.000000000000000000, -0.000000000000000000, -0.000000000000000000 ) ) ;
#10375 = B_SPLINE_CURVE_WITH_KNOTS ( 'NONE', 3,
 ( #9004, #2145, #9193, #5198, #8177, #11088, #6963, #314, #8939, #2217, #252, #2338, #11856, #9958, #377, #5322, #3228, #3289, #6020, #10970 ),
 .UNSPECIFIED., .F., .F.,
 ( 4, 2, 2, 2, 2, 2, 2, 2, 2, 4 ),
 ( 0.000000000000000000, 0.0009807944672943543635, 0.001961588934588708727, 0.002942383401883063524, 0.003923177869177417454, 0.004903972336471771817, 0.005884766803766127048, 0.006375164037413299893, 0.006865561271060473605, 0.007846355738354819295 ),
 .UNSPECIFIED. ) ;
#10376 = ORIENTED_EDGE ( 'NONE', *, *, #1394, .T. ) ;
#10377 = EDGE_CURVE ( 'NONE', #11047, #3445, #8736, .T. ) ;
#10378 = VECTOR ( 'NONE', #4260, 1000.000000000000000 ) ;
#10379 = CARTESIAN_POINT ( 'NONE',  ( 0.000000000000000000, 0.000000000000000000, 0.000000000000000000 ) ) ;
#10380 = PLANE ( 'NONE',  #2775 ) ;
#10381 = CARTESIAN_POINT ( 'NONE',  ( 39.77500000054622831, 20.00000000000000355, 98.07665518445361386 ) ) ;
#10382 = CARTESIAN_POINT ( 'NONE',  ( 40.37500000054621552, 12.34168156654572535, 90.79316153445363113 ) ) ;
#10383 = EDGE_CURVE ( 'NONE', #6436, #10421, #4762, .T. ) ;
#10384 = MANIFOLD_SOLID_BREP ( 'Hex', #8496 ) ;
#10385 = CARTESIAN_POINT ( 'NONE',  ( 20.77500000054622831, 20.00000000000000355, 83.50966788445364841 ) ) ;
#10386 = CARTESIAN_POINT ( 'NONE',  ( 10.00000000000000355, 20.00000000000000355, 69.99999999999998579 ) ) ;
#10387 = CARTESIAN_POINT ( 'NONE',  ( -50.00000000000001421, 18.00000000000000355, 188.4007504869563263 ) ) ;
#10388 = CIRCLE ( 'NONE', #870, 23.49999999999999289 ) ;
#10389 = CARTESIAN_POINT ( 'NONE',  ( 35.89999999999999147, 22.43689772174678154, 98.29316153445364534 ) ) ;
#10390 = FACE_OUTER_BOUND ( 'NONE', #7532, .T. ) ;
#10391 = EDGE_CURVE ( 'NONE', #4807, #6993, #5010, .T. ) ;
#10392 = DIRECTION ( 'NONE',  ( -1.000000000000000000, -0.000000000000000000, -0.000000000000000000 ) ) ;
#10393 = ORIENTED_EDGE ( 'NONE', *, *, #1693, .F. ) ;
#10394 = LINE ( 'NONE', #2725, #5306 ) ;
#10395 = CARTESIAN_POINT ( 'NONE',  ( 68.81432521710080152, 20.00000000000000000, 144.9999999999999716 ) ) ;
#10396 = VECTOR ( 'NONE', #249, 1000.000000000000000 ) ;
#10397 = EDGE_CURVE ( 'NONE', #6466, #3859, #7143, .T. ) ;
#10398 = CARTESIAN_POINT ( 'NONE',  ( 27.45000000109246585, 24.40838939219354842, 96.86078899226572503 ) ) ;
#10399 = CARTESIAN_POINT ( 'NONE',  ( 37.07500000054621836, 26.19570976099943849, 86.29171490190961435 ) ) ;
#10400 = CARTESIAN_POINT ( 'NONE',  ( 30.77500000054621765, 17.63344945572770328, 83.50966788445364841 ) ) ;
#10401 = CARTESIAN_POINT ( 'NONE',  ( 30.89999999999998437, 17.56310227825321135, 83.29316153445363113 ) ) ;
#10402 = CARTESIAN_POINT ( 'NONE',  ( -2.631691148149290171, 29.67035037513104712, 20.84471558130442759 ) ) ;
#10403 = CARTESIAN_POINT ( 'NONE',  ( 41.77500000054622831, 20.00000000000000355, 98.07665518445361386 ) ) ;
#10404 = ORIENTED_EDGE ( 'NONE', *, *, #8301, .T. ) ;
#10405 = CARTESIAN_POINT ( 'NONE',  ( 20.75000000109246656, 22.43689772174679575, 83.29316153445363113 ) ) ;
#10406 = CARTESIAN_POINT ( 'NONE',  ( -0.6587939304379992755, 45.03274104319341120, -20.99213535553697341 ) ) ;
#10407 = ORIENTED_EDGE ( 'NONE', *, *, #833, .T. ) ;
#10408 = AXIS2_PLACEMENT_3D ( 'NONE', #7951, #5983, #22 ) ;
#10409 = CARTESIAN_POINT ( 'NONE',  ( -3.230287074538311654, 29.46960489198576383, -27.81483967107842403 ) ) ;
#10410 = ORIENTED_EDGE ( 'NONE', *, *, #10533, .F. ) ;
#10411 = CARTESIAN_POINT ( 'NONE',  ( 2.611671490993349831, 29.65850121673988227, -24.86521292532985328 ) ) ;
#10412 = CARTESIAN_POINT ( 'NONE',  ( 23.10660171779821326, 27.49999999999999645, 140.6066017177982133 ) ) ;
#10413 = DIRECTION ( 'NONE',  ( 1.000000000000000000, -0.000000000000000000, -0.000000000000000000 ) ) ;
#10414 = CARTESIAN_POINT ( 'NONE',  ( 42.87500000054622262, 20.00000000000000355, 83.50966788445364841 ) ) ;
#10415 = DIRECTION ( 'NONE',  ( 0.000000000000000000, 0.000000000000000000, -1.000000000000000000 ) ) ;
#10416 = CARTESIAN_POINT ( 'NONE',  ( 46.37500000054621552, 12.34168156654572535, 90.79316153445363113 ) ) ;
#10417 = CARTESIAN_POINT ( 'NONE',  ( 46.39999999999999147, 12.86707612778636012, 93.11078899226572503 ) ) ;
#10418 = CIRCLE ( 'NONE', #1115, 7.499999999999978684 ) ;
#10419 = CARTESIAN_POINT ( 'NONE',  ( -10.00000000000000355, 20.00000000000000355, -28.00000000000000711 ) ) ;
#10420 = CARTESIAN_POINT ( 'NONE',  ( 39.65000000109246514, 20.00000000000000355, 98.29316153445363113 ) ) ;
#10421 = VERTEX_POINT ( 'NONE', #9248 ) ;
#10422 = CARTESIAN_POINT ( 'NONE',  ( 34.75000000109245235, 22.43689772174679575, 83.29316153445363113 ) ) ;
#10423 = EDGE_LOOP ( 'NONE', ( #860, #6148, #4000, #1031, #7042, #2545, #5482, #10608, #8527, #11220, #10489, #8648, #5057, #5348, #3082, #7306 ) ) ;
#10424 = CARTESIAN_POINT ( 'NONE',  ( -2.000000000000015543, 20.00000000000000355, 90.79316153445363113 ) ) ;
#10425 = ORIENTED_EDGE ( 'NONE', *, *, #8947, .F. ) ;
#10426 = CARTESIAN_POINT ( 'NONE',  ( -5.300214471940789096, 11.51392236371535382, -24.43326627631521220 ) ) ;
#10427 = VECTOR ( 'NONE', #12468, 1000.000000000000000 ) ;
#10428 = MANIFOLD_SOLID_BREP ( 'Hex', #798 ) ;
#10429 = CARTESIAN_POINT ( 'NONE',  ( -50.00000000000001421, 20.00000000000000000, 145.0000000000000000 ) ) ;
#10430 = CARTESIAN_POINT ( 'NONE',  ( -0.3295322344531997905, 30.00000000000001066, 25.00000000000001066 ) ) ;
#10431 = DIRECTION ( 'NONE',  ( -1.000000000000000000, -0.000000000000000000, -0.000000000000000000 ) ) ;
#10432 = CARTESIAN_POINT ( 'NONE',  ( -1.302025784688028764, 45.16141512708880867, 20.96206104378117985 ) ) ;
#10433 = DIRECTION ( 'NONE',  ( 0.000000000000000000, 1.000000000000000000, 0.000000000000000000 ) ) ;
#10434 = CARTESIAN_POINT ( 'NONE',  ( -2.612894974895984213, 10.32515758870095546, 27.88526400371763003 ) ) ;
#10435 = CARTESIAN_POINT ( 'NONE',  ( 20.87500000054622973, 22.36655054427230382, 83.50966788445364841 ) ) ;
#10436 = ADVANCED_FACE ( 'NONE', ( #4415 ), #11141, .T. ) ;
#10437 = FACE_BOUND ( 'NONE', #10257, .T. ) ;
#10438 = CARTESIAN_POINT ( 'NONE',  ( -5.000000000000000000, 50.32679387323496911, 24.49489742783177704 ) ) ;
#10439 = ORIENTED_EDGE ( 'NONE', *, *, #4904, .T. ) ;
#10440 = ORIENTED_EDGE ( 'NONE', *, *, #1553, .F. ) ;
#10441 = CARTESIAN_POINT ( 'NONE',  ( -10.00000000000000355, 20.00000000000000355, -18.46618531261938401 ) ) ;
#10442 = DIRECTION ( 'NONE',  ( 1.000000000000000000, 0.000000000000000000, 0.000000000000000000 ) ) ;
#10443 = CARTESIAN_POINT ( 'NONE',  ( 35.17500000054621268, 26.19570976099943493, 86.29171490190961435 ) ) ;
#10444 = CARTESIAN_POINT ( 'NONE',  ( 23.07500000054622902, 26.19570976099943849, 86.29171490190961435 ) ) ;
#10445 = DIRECTION ( 'NONE',  ( 0.000000000000000000, 0.000000000000000000, 1.000000000000000000 ) ) ;
#10446 = CARTESIAN_POINT ( 'NONE',  ( 4.338021161404794768, 47.49236434914906368, 24.62144314154611990 ) ) ;
#10447 = CARTESIAN_POINT ( 'NONE',  ( -5.000000000000000000, 50.00000000000000000, -20.39607805437114152 ) ) ;
#10448 = DIRECTION ( 'NONE',  ( 0.000000000000000000, 0.000000000000000000, 1.000000000000000000 ) ) ;
#10449 = DIRECTION ( 'NONE',  ( -0.7071067811865386910, 0.000000000000000000, 0.7071067811865564545 ) ) ;
#10450 = CARTESIAN_POINT ( 'NONE',  ( 3.429011037612589276E-15, 67.00000000000000000, 28.00000000000000000 ) ) ;
#10451 = ORIENTED_EDGE ( 'NONE', *, *, #5410, .T. ) ;
#10452 = DIRECTION ( 'NONE',  ( 0.000000000000000000, 0.000000000000000000, 1.000000000000000000 ) ) ;
#10453 = ADVANCED_FACE ( 'NONE', ( #6138, #10010 ), #9060, .T. ) ;
#10454 = DIRECTION ( 'NONE',  ( -1.000000000000000000, 0.000000000000000000, 0.000000000000000000 ) ) ;
#10455 = TOROIDAL_SURFACE ( 'NONE', #10658, 6.600000000000003197, 0.5999999999999999778 ) ;
#10456 = CARTESIAN_POINT ( 'NONE',  ( 24.47500000054622404, 13.07298590277314432, 88.54243821818161564 ) ) ;
#10457 = CARTESIAN_POINT ( 'NONE',  ( 36.39999999999999147, 12.86707612778636012, 93.11078899226572503 ) ) ;
#10458 = CARTESIAN_POINT ( 'NONE',  ( 42.47500000054622404, 13.80429023900056684, 86.29171490190961435 ) ) ;
#10459 = CARTESIAN_POINT ( 'NONE',  ( 28.27500000054622475, 13.07298590277314254, 93.04388485072563242 ) ) ;
#10460 = CARTESIAN_POINT ( 'NONE',  ( 28.19999999999998863, 15.59161060780645691, 96.86078899226572503 ) ) ;
#10461 = DIRECTION ( 'NONE',  ( 0.000000000000000000, 0.000000000000000000, 1.000000000000000000 ) ) ;
#10462 = CARTESIAN_POINT ( 'NONE',  ( 37.17500000054622689, 26.92701409722686634, 88.54243821818162985 ) ) ;
#10463 = ORIENTED_EDGE ( 'NONE', *, *, #8117, .T. ) ;
#10464 = CARTESIAN_POINT ( 'NONE',  ( 47.77500000054622831, 20.00000000000000355, 98.07665518445361386 ) ) ;
#10465 = CARTESIAN_POINT ( 'NONE',  ( -1.302315535602271757, 45.16144182297183107, -20.96205453846774347 ) ) ;
#10466 =( GEOMETRIC_REPRESENTATION_CONTEXT ( 3 ) GLOBAL_UNCERTAINTY_ASSIGNED_CONTEXT ( ( #2897 ) ) GLOBAL_UNIT_ASSIGNED_CONTEXT ( ( #431, #3467, #1447 ) ) REPRESENTATION_CONTEXT ( 'NONE', 'WORKASPACE' ) );
#10467 = VERTEX_POINT ( 'NONE', #1788 ) ;
#10468 = EDGE_CURVE ( 'NONE', #8006, #2800, #6798, .T. ) ;
#10469 = FACE_OUTER_BOUND ( 'NONE', #9865, .T. ) ;
#10470 = ORIENTED_EDGE ( 'NONE', *, *, #2346, .T. ) ;
#10471 = CARTESIAN_POINT ( 'NONE',  ( 0.6684871184501431918, 29.98311267939276092, -24.99323153604321490 ) ) ;
#10472 = CYLINDRICAL_SURFACE ( 'NONE', #9649, 7.499999999999992895 ) ;
#10473 = PLANE ( 'NONE',  #8656 ) ;
#10474 = CARTESIAN_POINT ( 'NONE',  ( 44.67500000054621978, 15.71886984736413773, 84.90069139318163138 ) ) ;
#10475 = LINE ( 'NONE', #3629, #3718 ) ;
#10476 = EDGE_CURVE ( 'NONE', #12073, #12014, #8764, .T. ) ;
#10477 = CIRCLE ( 'NONE', #2785, 8.400000000000000355 ) ;
#10478 = FACE_OUTER_BOUND ( 'NONE', #8608, .T. ) ;
#10479 = CARTESIAN_POINT ( 'NONE',  ( 43.07500000054622546, 24.28113015263587471, 84.90069139318163138 ) ) ;
#10480 = CARTESIAN_POINT ( 'NONE',  ( 20.27500000054622475, 13.07298590277314254, 93.04388485072563242 ) ) ;
#10481 = DIRECTION ( 'NONE',  ( 0.000000000000000000, 0.000000000000000000, -1.000000000000000000 ) ) ;
#10482 = DIRECTION ( 'NONE',  ( 0.000000000000000000, 0.000000000000000000, -1.000000000000000000 ) ) ;
#10483 = ORIENTED_EDGE ( 'NONE', *, *, #6380, .T. ) ;
#10484 = CARTESIAN_POINT ( 'NONE',  ( 35.05000000109246372, 27.13292387221364876, 88.47553407664153724 ) ) ;
#10485 = CARTESIAN_POINT ( 'NONE',  ( 12.59999999999999964, 0.000000000000000000, 0.000000000000000000 ) ) ;
#10486 = VERTEX_POINT ( 'NONE', #5733 ) ;
#10487 = DIRECTION ( 'NONE',  ( 0.000000000000000000, 0.5000000000000011102, 0.8660254037844379305 ) ) ;
#10488 = ADVANCED_FACE ( 'NONE', ( #975 ), #6863, .F. ) ;
#10489 = ORIENTED_EDGE ( 'NONE', *, *, #9256, .F. ) ;
#10490 = CARTESIAN_POINT ( 'NONE',  ( -8.980220477185385519, 24.44733350940715866, -23.33298399582670157 ) ) ;
#10491 = CYLINDRICAL_SURFACE ( 'NONE', #8262, 7.499999999999978684 ) ;
#10492 = DIRECTION ( 'NONE',  ( 0.7071067811865500152, 0.000000000000000000, 0.7071067811865451302 ) ) ;
#10493 = CONICAL_SURFACE ( 'NONE', #3801, 6.999999999999978684, 0.7853981633974473908 ) ;
#10494 = DIRECTION ( 'NONE',  ( -0.000000000000000000, -0.000000000000000000, 1.000000000000000000 ) ) ;
#10495 = CARTESIAN_POINT ( 'NONE',  ( -3.768782163415854036, 46.69792565062278555, 20.66038494228472899 ) ) ;
#10496 = ORIENTED_EDGE ( 'NONE', *, *, #5601, .F. ) ;
#10497 = COLOUR_RGB ( '',0.7921568627450980005, 0.8196078431372548767, 0.9333333333333333481 ) ;
#10498 = DIRECTION ( 'NONE',  ( 0.000000000000000000, 0.000000000000000000, 1.000000000000000000 ) ) ;
#10499 = FACE_OUTER_BOUND ( 'NONE', #12276, .T. ) ;
#10500 = CARTESIAN_POINT ( 'NONE',  ( 22.87500000054623328, 22.36655054427230382, 83.50966788445364841 ) ) ;
#10501 = FACE_OUTER_BOUND ( 'NONE', #7311, .T. ) ;
#10502 = ORIENTED_EDGE ( 'NONE', *, *, #9256, .T. ) ;
#10503 = VECTOR ( 'NONE', #3029, 1000.000000000000000 ) ;
#10504 = VERTEX_POINT ( 'NONE', #1910 ) ;
#10505 = EDGE_CURVE ( 'NONE', #5816, #10732, #4806, .T. ) ;
#10506 = B_SPLINE_CURVE_WITH_KNOTS ( 'NONE', 3,
 ( #3286, #9889, #10698, #6141, #2011, #1259, #6015, #8110, #3030, #9762, #8997, #4238, #6083, #10760, #10966, #9953, #310, #1202, #6895, #1138, #7919, #2140, #5891, #2211 ),
 .UNSPECIFIED., .F., .F.,
 ( 4, 2, 2, 2, 2, 2, 2, 2, 2, 2, 2, 4 ),
 ( 0.04760885841731214013, 0.04859922075612807535, 0.04958958309494400363, 0.05157030777257586712, 0.05256067011139180234, 0.05355103245020773062, 0.05553175712783959411, 0.05751248180547145761, 0.05850284414428739282, 0.05949320648310332110, 0.06147393116073518460, 0.06345465583836705503 ),
 .UNSPECIFIED. ) ;
#10507 = CARTESIAN_POINT ( 'NONE',  ( -50.00000000000001421, 18.00000000000000355, 169.9999999999999716 ) ) ;
#10508 = CARTESIAN_POINT ( 'NONE',  ( 6.000000000000000000, -5.839897972853060892, 7.806255641895631925E-15 ) ) ;
#10509 = MECHANICAL_DESIGN_GEOMETRIC_PRESENTATION_REPRESENTATION (  '', ( #1005 ), #8290 ) ;
#10510 = DIRECTION ( 'NONE',  ( -1.000000000000000000, 0.000000000000000000, 0.000000000000000000 ) ) ;
#10511 = DIRECTION ( 'NONE',  ( 0.000000000000000000, 0.000000000000000000, -1.000000000000000000 ) ) ;
#10512 = LINE ( 'NONE', #878, #3313 ) ;
#10513 = CARTESIAN_POINT ( 'NONE',  ( 4.741665211587190676, 48.38057902784014175, 27.59588127970951632 ) ) ;
#10514 = CARTESIAN_POINT ( 'NONE',  ( 4.450527323037263727, 11.02130320606087821, 24.60818795580814822 ) ) ;
#10515 = ORIENTED_EDGE ( 'NONE', *, *, #7992, .F. ) ;
#10516 = DIRECTION ( 'NONE',  ( -0.000000000000000000, -0.000000000000000000, 1.000000000000000000 ) ) ;
#10517 = DIRECTION ( 'NONE',  ( 0.000000000000000000, 0.8153487308096339925, 0.5789701608607470407 ) ) ;
#10518 = CARTESIAN_POINT ( 'NONE',  ( 27.27500000054622475, 26.92701409722686634, 88.54243821818162985 ) ) ;
#10519 = CARTESIAN_POINT ( 'NONE',  ( 28.85000000109246443, 24.40838939219355197, 84.72553407664153724 ) ) ;
#10520 = CARTESIAN_POINT ( 'NONE',  ( 42.37500000054622262, 13.07298590277314432, 88.54243821818161564 ) ) ;
#10521 = CARTESIAN_POINT ( 'NONE',  ( 30.47500000054622404, 13.07298590277314432, 88.54243821818161564 ) ) ;
#10522 = CARTESIAN_POINT ( 'NONE',  ( 32.29999999999999005, 13.62011893735971135, 95.42841645007781892 ) ) ;
#10523 = EDGE_CURVE ( 'NONE', #10579, #11516, #7755, .T. ) ;
#10524 = CARTESIAN_POINT ( 'NONE',  ( -50.00000000000001421, 0.000000000000000000, 121.2488769092545198 ) ) ;
#10525 = CARTESIAN_POINT ( 'NONE',  ( 31.27500000054622831, 27.65831843345427998, 90.79316153445363113 ) ) ;
#10526 = VERTEX_POINT ( 'NONE', #3881 ) ;
#10527 = CIRCLE ( 'NONE', #5077, 0.5999999999999998668 ) ;
#10528 = CARTESIAN_POINT ( 'NONE',  ( 48.67500000054623399, 17.63344945572770328, 83.50966788445364841 ) ) ;
#10529 = CARTESIAN_POINT ( 'NONE',  ( 28.15000000109246159, 12.11403331821300533, 90.79316153445363113 ) ) ;
#10530 = EDGE_LOOP ( 'NONE', ( #999, #8465, #10626, #9069, #3242 ) ) ;
#10531 = PRODUCT_DEFINITION ( 'UNKNOWN', '', #888, #10942 ) ;
#10532 = CARTESIAN_POINT ( 'NONE',  ( -4.140053538423851224E-16, 30.00000000000001066, -28.00000000000000355 ) ) ;
#10533 = EDGE_CURVE ( 'NONE', #332, #4818, #10664, .T. ) ;
#10534 = ORIENTED_EDGE ( 'NONE', *, *, #6444, .F. ) ;
#10535 = CARTESIAN_POINT ( 'NONE',  ( 9.466290622766221574, 23.23991477998078636, -23.13871526284164304 ) ) ;
#10536 = CARTESIAN_POINT ( 'NONE',  ( 32.09999999999998721, 17.56310227825320425, 98.29316153445363113 ) ) ;
#10537 = FACE_OUTER_BOUND ( 'NONE', #4062, .T. ) ;
#10538 = VECTOR ( 'NONE', #3983, 1000.000000000000000 ) ;
#10539 = CARTESIAN_POINT ( 'NONE',  ( 47.37500000054622262, 27.65831843345427998, 90.79316153445363113 ) ) ;
#10540 = CARTESIAN_POINT ( 'NONE',  ( 52.99999999999998579, 20.00000000000000355, 169.9999999999999716 ) ) ;
#10541 = DIRECTION ( 'NONE',  ( -0.000000000000000000, -1.000000000000000000, -0.000000000000000000 ) ) ;
#10542 = CARTESIAN_POINT ( 'NONE',  ( 42.57500000054622546, 13.80429023900056684, 86.29171490190961435 ) ) ;
#10543 = CARTESIAN_POINT ( 'NONE',  ( 19.97500000054622404, 17.63344945572769973, 98.07665518445361386 ) ) ;
#10544 = CARTESIAN_POINT ( 'NONE',  ( -6.108719317430274742, 27.92396576624410187, -24.24357326025485193 ) ) ;
#10545 = CARTESIAN_POINT ( 'NONE',  ( 0.000000000000000000, 20.00000000000000355, 109.9999999999999858 ) ) ;
#10546 = ORIENTED_EDGE ( 'NONE', *, *, #6826, .T. ) ;
#10547 = CARTESIAN_POINT ( 'NONE',  ( 39.05000000109247082, 27.13292387221364876, 88.47553407664153724 ) ) ;
#10548 = DIRECTION ( 'NONE',  ( 0.000000000000000000, 0.000000000000000000, -1.000000000000000000 ) ) ;
#10549 = EDGE_LOOP ( 'NONE', ( #2702, #1999, #1037, #10981, #6853 ) ) ;
#10550 = DIRECTION ( 'NONE',  ( 0.000000000000000000, 0.8660254037844380415, -0.5000000000000012212 ) ) ;
#10551 = VECTOR ( 'NONE', #6856, 1000.000000000000000 ) ;
#10552 = EDGE_CURVE ( 'NONE', #1942, #7750, #6671, .T. ) ;
#10553 = ORIENTED_EDGE ( 'NONE', *, *, #9100, .F. ) ;
#10554 = CARTESIAN_POINT ( 'NONE',  ( 0.000000000000000000, -3.000000000000003109, 0.000000000000000000 ) ) ;
#10555 = LINE ( 'NONE', #12285, #3397 ) ;
#10556 = CARTESIAN_POINT ( 'NONE',  ( -5.025242304149237782, 28.65182443915274746, 24.49149081028624053 ) ) ;
#10557 = ADVANCED_FACE ( 'NONE', ( #10478 ), #7634, .F. ) ;
#10558 = DIRECTION ( 'NONE',  ( 1.000000000000000000, 0.000000000000000000, 0.000000000000000000 ) ) ;
#10559 = CARTESIAN_POINT ( 'NONE',  ( 28.00000000000000711, -3.000000000000003109, 0.000000000000000000 ) ) ;
#10560 = EDGE_LOOP ( 'NONE', ( #5226, #6696, #10999, #2164, #6927 ) ) ;
#10561 = CARTESIAN_POINT ( 'NONE',  ( 4.968243444659302455, 50.65191788982895815, -27.55577634755498906 ) ) ;
#10562 = CARTESIAN_POINT ( 'NONE',  ( 47.75000000109246656, 17.56310227825322556, 98.29316153445364534 ) ) ;
#10563 = CARTESIAN_POINT ( 'NONE',  ( 21.97500000054622760, 15.71886984736413417, 96.68563167572563088 ) ) ;
#10564 = ORIENTED_EDGE ( 'NONE', *, *, #7493, .T. ) ;
#10565 = CARTESIAN_POINT ( 'NONE',  ( 45.95000000109245519, 13.62011893735970958, 95.42841645007781892 ) ) ;
#10566 = CARTESIAN_POINT ( 'NONE',  ( 5.000000000000000000, 50.32977410740986812, -20.39607805437114152 ) ) ;
#10567 = ORIENTED_EDGE ( 'NONE', *, *, #1653, .T. ) ;
#10568 = ORIENTED_EDGE ( 'NONE', *, *, #1801, .F. ) ;
#10569 = CARTESIAN_POINT ( 'NONE',  ( -8.670263310646999955, 25.02480281026656073, -19.13064292386552268 ) ) ;
#10570 = CARTESIAN_POINT ( 'NONE',  ( 0.000000000000000000, 0.000000000000000000, 0.000000000000000000 ) ) ;
#10571 = MANIFOLD_SOLID_BREP ( 'Chamfer3', #6063 ) ;
#10572 = EDGE_CURVE ( 'NONE', #3577, #10746, #8214, .T. ) ;
#10573 = LINE ( 'NONE', #8554, #11450 ) ;
#10574 = CARTESIAN_POINT ( 'NONE',  ( 6.000000000000000000, -5.839897972853060892, 7.806255641895631925E-15 ) ) ;
#10575 = CARTESIAN_POINT ( 'NONE',  ( 12.00000000000000000, 8.082668874372531019E-16, 6.599999999999999645 ) ) ;
#10576 = CARTESIAN_POINT ( 'NONE',  ( 3.303977982198811780, 46.23303585118835457, -20.73977949246337005 ) ) ;
#10577 = DIRECTION ( 'NONE',  ( -0.000000000000000000, -0.000000000000000000, 1.000000000000000000 ) ) ;
#10578 = CARTESIAN_POINT ( 'NONE',  ( -2.000000000000015543, 20.00000000000000355, 90.79316153445363113 ) ) ;
#10579 = VERTEX_POINT ( 'NONE', #10726 ) ;
#10580 = B_SPLINE_CURVE_WITH_KNOTS ( 'NONE', 3,
 ( #4098, #6010, #4166, #9883, #10134, #8039, #10070, #2204, #12032, #8103, #3337, #3150, #9945, #7201, #1380, #427, #1319, #11910, #11077, #2385, #1254, #1444, #2268, #8988, #5125, #6136, #10007, #5189 ),
 .UNSPECIFIED., .F., .F.,
 ( 4, 2, 2, 2, 2, 2, 2, 2, 2, 2, 2, 2, 2, 4 ),
 ( 0.01588527608562245730, 0.01687704675167533280, 0.01786881741772820831, 0.01886058808378108381, 0.01985235874983395932, 0.02183590008193970339, 0.02282767074799257542, 0.02381944141404544746, 0.02580298274615118459, 0.02679475341220405663, 0.02778652407825692866, 0.02877829474430979723, 0.02977006541036266579, 0.03175360674246840986 ),
 .UNSPECIFIED. ) ;
#10581 = ITEM_DEFINED_TRANSFORMATION ( 'NONE', 'NONE', #11421,  #9021 ) ;
#10582 = CARTESIAN_POINT ( 'NONE',  ( 47.87500000054622262, 20.00000000000000355, 98.07665518445361386 ) ) ;
#10583 = AXIS2_PLACEMENT_3D ( 'NONE', #6280, #386, #11038 ) ;
#10584 = CARTESIAN_POINT ( 'NONE',  ( 39.07500000054621836, 26.19570976099943849, 86.29171490190961435 ) ) ;
#10585 = CARTESIAN_POINT ( 'NONE',  ( 30.57500000054622191, 13.80429023900056684, 86.29171490190961435 ) ) ;
#10586 = CARTESIAN_POINT ( 'NONE',  ( 31.59999999999999076, 27.13292387221364876, 93.11078899226573924 ) ) ;
#10587 = CARTESIAN_POINT ( 'NONE',  ( 30.57500000054622902, 15.71886984736413773, 84.90069139318163138 ) ) ;
#10588 = ORIENTED_EDGE ( 'NONE', *, *, #396, .T. ) ;
#10589 = CARTESIAN_POINT ( 'NONE',  ( 3.024050948510435495E-21, 45.00000000000000711, -21.00000000000000000 ) ) ;
#10590 = VERTEX_POINT ( 'NONE', #2039 ) ;
#10591 = EDGE_CURVE ( 'NONE', #11427, #1348, #2944, .T. ) ;
#10592 = CARTESIAN_POINT ( 'NONE',  ( 0.000000000000000000, 67.00000000000000000, -28.00000000000000000 ) ) ;
#10593 = ORIENTED_EDGE ( 'NONE', *, *, #5340, .T. ) ;
#10594 = CARTESIAN_POINT ( 'NONE',  ( 32.79999999999999005, 15.59161060780646046, 84.72553407664153724 ) ) ;
#10595 = LINE ( 'NONE', #2035, #2584 ) ;
#10596 = CARTESIAN_POINT ( 'NONE',  ( 47.17500000054622689, 26.19570976099943849, 86.29171490190961435 ) ) ;
#10597 = CARTESIAN_POINT ( 'NONE',  ( 41.65000000109246514, 20.00000000000000355, 98.29316153445363113 ) ) ;
#10598 = CARTESIAN_POINT ( 'NONE',  ( 21.47500000054622404, 26.92701409722686634, 93.04388485072563242 ) ) ;
#10599 = VECTOR ( 'NONE', #2885, 1000.000000000000000 ) ;
#10600 = CARTESIAN_POINT ( 'NONE',  ( 45.19999999999998863, 24.40838939219355197, 84.72553407664153724 ) ) ;
#10601 = DIRECTION ( 'NONE',  ( -0.000000000000000000, -0.000000000000000000, 1.000000000000000000 ) ) ;
#10602 = ORIENTED_EDGE ( 'NONE', *, *, #2420, .T. ) ;
#10603 = AXIS2_PLACEMENT_3D ( 'NONE', #7357, #11417, #9459 ) ;
#10604 = CARTESIAN_POINT ( 'NONE',  ( 34.15000000109245804, 12.11403331821300533, 90.79316153445363113 ) ) ;
#10605 = CARTESIAN_POINT ( 'NONE',  ( -20.00000000000001776, 20.00000000000000000, 137.5000000000000000 ) ) ;
#10606 = ORIENTED_EDGE ( 'NONE', *, *, #11334, .F. ) ;
#10607 = CARTESIAN_POINT ( 'NONE',  ( -5.000000000000000888, 22.00000000000000000, 218.7511230907454944 ) ) ;
#10608 = ORIENTED_EDGE ( 'NONE', *, *, #8399, .T. ) ;
#10609 = LINE ( 'NONE', #9554, #4243 ) ;
#10610 = EDGE_CURVE ( 'NONE', #10486, #1560, #4070, .T. ) ;
#10611 = CARTESIAN_POINT ( 'NONE',  ( 3.258993009127279628, 10.52298990541062551, -20.75479906574401667 ) ) ;
#10612 = AXIS2_PLACEMENT_3D ( 'NONE', #619, #11023, #497 ) ;
#10613 = CARTESIAN_POINT ( 'NONE',  ( -2.619138840591237472, 29.67330545628644600, 24.87083797681799169 ) ) ;
#10614 =( BOUNDED_CURVE ( )  B_SPLINE_CURVE ( 3, ( #5708, #7480, #6772, #9637 ),
 .UNSPECIFIED., .F., .F. ) 
 B_SPLINE_CURVE_WITH_KNOTS ( ( 4, 4 ),
 ( 0.000000000000000000, 1.570796326794896558 ),
 .UNSPECIFIED. ) 
 CURVE ( )  GEOMETRIC_REPRESENTATION_ITEM ( )  RATIONAL_B_SPLINE_CURVE ( ( 1.000000000000000000, 0.8047378541243649375, 0.8047378541243649375, 1.000000000000000000 ) ) 
 REPRESENTATION_ITEM ( '' )  );
#10615 = CARTESIAN_POINT ( 'NONE',  ( 40.17500000054623399, 13.07298590277314254, 93.04388485072563242 ) ) ;
#10616 = CARTESIAN_POINT ( 'NONE',  ( 35.15000000109246514, 27.88596668178699645, 90.79316153445363113 ) ) ;
#10617 = DIRECTION ( 'NONE',  ( 0.000000000000000000, 0.000000000000000000, 1.000000000000000000 ) ) ;
#10618 = CARTESIAN_POINT ( 'NONE',  ( 34.35000000109246798, 13.62011893735970958, 86.15790661882942914 ) ) ;
#10619 = ORIENTED_EDGE ( 'NONE', *, *, #12308, .F. ) ;
#10620 = LINE ( 'NONE', #8543, #98 ) ;
#10621 = DIRECTION ( 'NONE',  ( 1.000000000000000000, -0.000000000000000000, -0.000000000000000000 ) ) ;
#10622 = CARTESIAN_POINT ( 'NONE',  ( 22.97500000054622760, 24.28113015263587471, 84.90069139318163138 ) ) ;
#10623 = ORIENTED_EDGE ( 'NONE', *, *, #1765, .T. ) ;
#10624 = CARTESIAN_POINT ( 'NONE',  ( -5.000000000000000000, 50.00000000000000000, -27.54995462791182703 ) ) ;
#10625 = DIRECTION ( 'NONE',  ( 1.000000000000000000, 0.000000000000000000, 0.000000000000000000 ) ) ;
#10626 = ORIENTED_EDGE ( 'NONE', *, *, #6521, .F. ) ;
#10627 = CIRCLE ( 'NONE', #5175, 25.00000000000000355 ) ;
#10628 = EDGE_CURVE ( 'NONE', #1878, #9719, #6922, .T. ) ;
#10629 = ORIENTED_EDGE ( 'NONE', *, *, #1474, .T. ) ;
#10630 = FACE_OUTER_BOUND ( 'NONE', #12348, .T. ) ;
#10631 = CARTESIAN_POINT ( 'NONE',  ( -27.49999999999999645, 12.50000000000001066, 145.0000000000000000 ) ) ;
#10632 = VECTOR ( 'NONE', #1226, 999.9999999999998863 ) ;
#10633 = EDGE_CURVE ( 'NONE', #1127, #9352, #6923, .T. ) ;
#10634 = PLANE ( 'NONE',  #2535 ) ;
#10635 = FACE_OUTER_BOUND ( 'NONE', #7371, .T. ) ;
#10636 = CARTESIAN_POINT ( 'NONE',  ( -4.680564368149037868, 51.76601715386365044, -20.47184426876964025 ) ) ;
#10637 = PLANE ( 'NONE',  #5341 ) ;
#10638 = CARTESIAN_POINT ( 'NONE',  ( 8.481410126304654185, 25.30750070271793817, -19.21207824733827252 ) ) ;
#10639 = VECTOR ( 'NONE', #7878, 1000.000000000000000 ) ;
#10640 = CARTESIAN_POINT ( 'NONE',  ( 9.465993554759519313, 16.75899710733777326, 23.13883973029316010 ) ) ;
#10641 = VERTEX_POINT ( 'NONE', #8077 ) ;
#10642 = CARTESIAN_POINT ( 'NONE',  ( 5.839560020365381021, 28.12428960229776465, -24.30998564924267313 ) ) ;
#10643 = CIRCLE ( 'NONE', #12283, 9.000000000000000000 ) ;
#10644 = SHAPE_DEFINITION_REPRESENTATION ( #7206, #3370 ) ;
#10645 = CARTESIAN_POINT ( 'NONE',  ( 23.65000000109246514, 20.00000000000000355, 98.29316153445363113 ) ) ;
#10646 = VECTOR ( 'NONE', #1163, 1000.000000000000000 ) ;
#10647 = CARTESIAN_POINT ( 'NONE',  ( 37.47500000054623115, 26.19570976099943849, 95.29460816699764791 ) ) ;
#10648 = CARTESIAN_POINT ( 'NONE',  ( 30.37500000054622618, 12.34168156654572535, 90.79316153445363113 ) ) ;
#10649 = CARTESIAN_POINT ( 'NONE',  ( 22.89999999999998792, 17.56310227825321135, 83.29316153445363113 ) ) ;
#10650 = DIRECTION ( 'NONE',  ( 1.000000000000000000, -0.000000000000000000, -0.000000000000000000 ) ) ;
#10651 = CARTESIAN_POINT ( 'NONE',  ( 32.47500000054623825, 13.80429023900056684, 86.29171490190961435 ) ) ;
#10652 = ORIENTED_EDGE ( 'NONE', *, *, #2428, .T. ) ;
#10653 = ADVANCED_FACE ( 'NONE', ( #4005 ), #9917, .F. ) ;
#10654 = CARTESIAN_POINT ( 'NONE',  ( 0.6000000000000033085, 0.000000000000000000, 9.000000000000000000 ) ) ;
#10655 = ORIENTED_EDGE ( 'NONE', *, *, #10591, .F. ) ;
#10656 = CARTESIAN_POINT ( 'NONE',  ( 6.000000000000000000, 0.000000000000000000, 5.057500000000000107 ) ) ;
#10657 = ORIENTED_EDGE ( 'NONE', *, *, #5886, .F. ) ;
#10658 = AXIS2_PLACEMENT_3D ( 'NONE', #505, #4368, #2523 ) ;
#10659 = CARTESIAN_POINT ( 'NONE',  ( 91.03600000000000136, 0.000000000000000000, 0.000000000000000000 ) ) ;
#10660 = FACE_OUTER_BOUND ( 'NONE', #266, .T. ) ;
#10661 = CARTESIAN_POINT ( 'NONE',  ( 43.97500000054622404, 17.63344945572769973, 98.07665518445361386 ) ) ;
#10662 = CARTESIAN_POINT ( 'NONE',  ( -5.000000000000000000, 50.00000000000000000, -28.00000000000000711 ) ) ;
#10663 = EDGE_CURVE ( 'NONE', #724, #1877, #12464, .T. ) ;
#10664 = LINE ( 'NONE', #12220, #11281 ) ;
#10665 = CARTESIAN_POINT ( 'NONE',  ( 44.57500000054622546, 13.80429023900056684, 86.29171490190961435 ) ) ;
#10666 = CARTESIAN_POINT ( 'NONE',  ( 40.09999999999998721, 17.56310227825320425, 98.29316153445363113 ) ) ;
#10667 = AXIS2_PLACEMENT_3D ( 'NONE', #11466, #2774, #7663 ) ;
#10668 = CARTESIAN_POINT ( 'NONE',  ( 40.59999999999998721, 12.86707612778636012, 88.47553407664152303 ) ) ;
#10669 = FACE_OUTER_BOUND ( 'NONE', #2049, .T. ) ;
#10670 = ORIENTED_EDGE ( 'NONE', *, *, #1394, .F. ) ;
#10671 = CARTESIAN_POINT ( 'NONE',  ( 34.45000000109246940, 15.59161060780646046, 84.72553407664153724 ) ) ;
#10672 = CARTESIAN_POINT ( 'NONE',  ( -6.999999999999999112, 92.00000000000000000, 69.99999999999998579 ) ) ;
#10673 = ORIENTED_EDGE ( 'NONE', *, *, #9978, .T. ) ;
#10674 = ORIENTED_EDGE ( 'NONE', *, *, #1701, .T. ) ;
#10675 = CARTESIAN_POINT ( 'NONE',  ( -9.935193375007562722, 21.31442233758455274, -22.94148538850174646 ) ) ;
#10676 = AXIS2_PLACEMENT_3D ( 'NONE', #5147, #1518, #9013 ) ;
#10677 = CARTESIAN_POINT ( 'NONE',  ( 2.571758278209441661E-15, 139.9999999999999716, 21.00000000000000000 ) ) ;
#10678 = CARTESIAN_POINT ( 'NONE',  ( -2.000000000000015543, 20.00000000000000355, 98.29316153445363113 ) ) ;
#10679 = CARTESIAN_POINT ( 'NONE',  ( 33.97500000054623115, 15.71886984736413417, 96.68563167572563088 ) ) ;
#10680 = CARTESIAN_POINT ( 'NONE',  ( 37.97500000054621694, 17.63344945572769973, 98.07665518445361386 ) ) ;
#10681 = CARTESIAN_POINT ( 'NONE',  ( 35.25000000109245946, 27.13292387221364876, 93.11078899226573924 ) ) ;
#10682 = CARTESIAN_POINT ( 'NONE',  ( 43.75000000109248077, 17.56310227825318648, 98.29316153445363113 ) ) ;
#10683 = ORIENTED_EDGE ( 'NONE', *, *, #2036, .F. ) ;
#10684 = EDGE_CURVE ( 'NONE', #852, #1585, #5635, .T. ) ;
#10685 = CARTESIAN_POINT ( 'NONE',  ( 1.500000000000001332, 7.960204194457796463E-16, -6.500000000000000888 ) ) ;
#10686 = CARTESIAN_POINT ( 'NONE',  ( 12.00000000000000178, 9.000000000000000000, 0.000000000000000000 ) ) ;
#10687 = ORIENTED_EDGE ( 'NONE', *, *, #1724, .T. ) ;
#10688 = DIRECTION ( 'NONE',  ( 0.000000000000000000, 1.000000000000000000, -1.110768649713241713E-15 ) ) ;
#10689 = ORIENTED_EDGE ( 'NONE', *, *, #12508, .T. ) ;
#10690 = VERTEX_POINT ( 'NONE', #8829 ) ;
#10691 = EDGE_CURVE ( 'NONE', #9799, #6453, #2966, .T. ) ;
#10692 =( BOUNDED_CURVE ( )  B_SPLINE_CURVE ( 2, ( #10043, #1354, #5220, #12435, #9524, #8624, #10457, #2730, #4692, #2788, #6650 ),
 .UNSPECIFIED., .F., .F. ) 
 B_SPLINE_CURVE_WITH_KNOTS ( ( 3, 2, 2, 2, 2, 3 ),
 ( 0.4333333333333332926, 0.4399999999999999467, 0.4466666666666666008, 0.4533333333333332549, 0.4599999999999999645, 0.4666666666666666186 ),
 .UNSPECIFIED. ) 
 CURVE ( )  GEOMETRIC_REPRESENTATION_ITEM ( )  RATIONAL_B_SPLINE_CURVE ( ( 1.000000000000000444, 0.9510565162951531981, 1.000000000000000000, 0.9510565162951535312, 1.000000000000000000, 0.9510565162951535312, 1.000000000000000000, 0.9510565162951535312, 1.000000000000000000, 0.9510565162951539753, 0.9999999999999995559 ) ) 
 REPRESENTATION_ITEM ( '' )  );
#10693 = VECTOR ( 'NONE', #9832, 999.9999999999998863 ) ;
#10694 = CARTESIAN_POINT ( 'NONE',  ( 42.75000000109245235, 22.43689772174680641, 83.29316153445363113 ) ) ;
#10695 = DIRECTION ( 'NONE',  ( 1.000000000000000000, -0.000000000000000000, -0.000000000000000000 ) ) ;
#10696 = CARTESIAN_POINT ( 'NONE',  ( 8.353307965316590256, 25.50093297180406182, 95.89657251760699808 ) ) ;
#10697 = CARTESIAN_POINT ( 'NONE',  ( 37.99999999999999289, 20.00000000000000355, 98.29316153445363113 ) ) ;
#10698 = CARTESIAN_POINT ( 'NONE',  ( 0.6606214661398540633, 29.98367637546362019, 20.99221177463937238 ) ) ;
#10699 = CARTESIAN_POINT ( 'NONE',  ( -20.27158385259951601, 22.00000000000000000, 169.9999999999999716 ) ) ;
#10700 = CARTESIAN_POINT ( 'NONE',  ( 6.000000000000000000, 0.000000000000000000, 0.000000000000000000 ) ) ;
#10701 = AXIS2_PLACEMENT_3D ( 'NONE', #11979, #433, #8296 ) ;
#10702 = CARTESIAN_POINT ( 'NONE',  ( 6.110979747148361341, 12.05740682582580625, 24.24803741642852373 ) ) ;
#10703 = ORIENTED_EDGE ( 'NONE', *, *, #6658, .F. ) ;
#10704 = CARTESIAN_POINT ( 'NONE',  ( 36.65000000109245804, 20.00000000000000355, 83.29316153445364534 ) ) ;
#10705 = EDGE_CURVE ( 'NONE', #4669, #10800, #7604, .T. ) ;
#10706 = ITEM_DEFINED_TRANSFORMATION ( 'NONE', 'NONE', #8381,  #9021 ) ;
#10707 = VECTOR ( 'NONE', #5780, 1000.000000000000000 ) ;
#10708 = CARTESIAN_POINT ( 'NONE',  ( 23.47500000054622404, 26.92701409722686634, 93.04388485072563242 ) ) ;
#10709 = CARTESIAN_POINT ( 'NONE',  ( 49.47500000054623115, 26.92701409722686634, 93.04388485072563242 ) ) ;
#10710 = CARTESIAN_POINT ( 'NONE',  ( 34.27500000054622831, 12.34168156654572357, 90.79316153445363113 ) ) ;
#10711 = EDGE_CURVE ( 'NONE', #11516, #2324, #10573, .T. ) ;
#10712 = CARTESIAN_POINT ( 'NONE',  ( 24.27500000054622475, 13.07298590277314254, 93.04388485072563242 ) ) ;
#10713 = CARTESIAN_POINT ( 'NONE',  ( 23.69999999999998508, 26.37988106264029398, 95.42841645007781892 ) ) ;
#10714 = CARTESIAN_POINT ( 'NONE',  ( 34.79999999999999005, 15.59161060780646046, 84.72553407664153724 ) ) ;
#10715 = CARTESIAN_POINT ( 'NONE',  ( 35.87500000054622262, 17.63344945572769973, 98.07665518445361386 ) ) ;
#10716 = ORIENTED_EDGE ( 'NONE', *, *, #3245, .T. ) ;
#10717 = CARTESIAN_POINT ( 'NONE',  ( 27.49999999999999645, 20.00000000000000355, 170.9999999999999716 ) ) ;
#10718 = ORIENTED_EDGE ( 'NONE', *, *, #7602, .F. ) ;
#10719 = CARTESIAN_POINT ( 'NONE',  ( 49.15000000109245804, 27.88596668178699645, 90.79316153445363113 ) ) ;
#10720 = ORIENTED_EDGE ( 'NONE', *, *, #958, .F. ) ;
#10721 =( LENGTH_UNIT ( ) NAMED_UNIT ( * ) SI_UNIT ( .MILLI., .METRE. ) );
#10722 = CARTESIAN_POINT ( 'NONE',  ( -4.839726511208201742, 51.29827509403275343, -24.52715513826036897 ) ) ;
#10723 = CARTESIAN_POINT ( 'NONE',  ( 0.3282094658107080343, 10.00000000000000000, -28.00000000000000355 ) ) ;
#10724 = CARTESIAN_POINT ( 'NONE',  ( 41.47500000054623115, 26.92701409722686634, 93.04388485072563242 ) ) ;
#10725 = DIRECTION ( 'NONE',  ( 0.000000000000000000, 0.000000000000000000, 1.000000000000000000 ) ) ;
#10726 = CARTESIAN_POINT ( 'NONE',  ( 5.000000000000000000, -4.685197434473812983, 6.938893903907228378E-15 ) ) ;
#10727 = CARTESIAN_POINT ( 'NONE',  ( 42.27500000054622120, 13.07298590277314254, 93.04388485072563242 ) ) ;
#10728 = CARTESIAN_POINT ( 'NONE',  ( 40.99999999999998579, 20.00000000000000355, 83.29316153445364534 ) ) ;
#10729 = AXIS2_PLACEMENT_3D ( 'NONE', #4060, #3872, #7938 ) ;
#10730 = CARTESIAN_POINT ( 'NONE',  ( 40.29999999999997584, 13.62011893735970958, 95.42841645007781892 ) ) ;
#10731 = PLANE ( 'NONE',  #5649 ) ;
#10732 = VERTEX_POINT ( 'NONE', #5705 ) ;
#10733 = CARTESIAN_POINT ( 'NONE',  ( 32.15000000109246514, 12.11403331821300533, 90.79316153445363113 ) ) ;
#10734 = CARTESIAN_POINT ( 'NONE',  ( 1.999999999999988010, 20.00000000000000355, 189.9999999999999716 ) ) ;
#10735 = ORIENTED_EDGE ( 'NONE', *, *, #1070, .T. ) ;
#10736 = ORIENTED_EDGE ( 'NONE', *, *, #5601, .T. ) ;
#10737 = AXIS2_PLACEMENT_3D ( 'NONE', #10269, #8497, #8374 ) ;
#10738 = CARTESIAN_POINT ( 'NONE',  ( -6.849710128414980836, 27.29284600759404356, -24.04449974210336904 ) ) ;
#10739 = PRODUCT_DEFINITION_SHAPE ( 'NONE', 'NONE',  #12546 ) ;
#10740 = DIRECTION ( 'NONE',  ( 0.000000000000000000, 0.000000000000000000, 1.000000000000000000 ) ) ;
#10741 = DIRECTION ( 'NONE',  ( 1.000000000000000000, -0.000000000000000000, -0.000000000000000000 ) ) ;
#10742 = CARTESIAN_POINT ( 'NONE',  ( 36.87500000054622973, 22.36655054427230382, 83.50966788445364841 ) ) ;
#10743 = CARTESIAN_POINT ( 'NONE',  ( 34.67500000054622689, 15.71886984736413773, 84.90069139318163138 ) ) ;
#10744 = CARTESIAN_POINT ( 'NONE',  ( 6.104805980962106915, 27.92701719664820459, -27.32760709691111956 ) ) ;
#10745 = DIRECTION ( 'NONE',  ( -1.000000000000000000, 0.000000000000000000, 0.000000000000000000 ) ) ;
#10746 = VERTEX_POINT ( 'NONE', #9634 ) ;
#10747 = CIRCLE ( 'NONE', #8734, 5.035999999999999588 ) ;
#10748 = CARTESIAN_POINT ( 'NONE',  ( 47.95000000109246230, 13.62011893735971135, 95.42841645007781892 ) ) ;
#10749 = CARTESIAN_POINT ( 'NONE',  ( 12.00000000000000355, 0.000000000000000000, 0.000000000000000000 ) ) ;
#10750 = ORIENTED_EDGE ( 'NONE', *, *, #10317, .F. ) ;
#10751 = CARTESIAN_POINT ( 'NONE',  ( 91.03600000000000136, 7.347880794884117764E-16, -5.999999999999998224 ) ) ;
#10752 = ORIENTED_EDGE ( 'NONE', *, *, #1189, .T. ) ;
#10753 = EDGE_CURVE ( 'NONE', #12336, #6828, #9633, .T. ) ;
#10754 = VERTEX_POINT ( 'NONE', #943 ) ;
#10755 = VECTOR ( 'NONE', #9335, 1000.000000000000114 ) ;
#10756 = CARTESIAN_POINT ( 'NONE',  ( 44.99999999999996447, 20.00000000000000355, 172.0000000000000000 ) ) ;
#10757 = CARTESIAN_POINT ( 'NONE',  ( 6.000000000000000000, -5.839897972853060892, 7.806255641895631925E-15 ) ) ;
#10758 = CARTESIAN_POINT ( 'NONE',  ( 8.665435081250036475, 25.00622661766839627, 96.39744239336449994 ) ) ;
#10759 = CARTESIAN_POINT ( 'NONE',  ( 37.19999999999998863, 24.40838939219355197, 84.72553407664153724 ) ) ;
#10760 = CARTESIAN_POINT ( 'NONE',  ( 7.535696908431325447, 26.60561170258834807, 19.60740232376276637 ) ) ;
#10761 = CARTESIAN_POINT ( 'NONE',  ( 5.000000000000000888, 50.00000000000000000, -20.39607805437114152 ) ) ;
#10762 = CARTESIAN_POINT ( 'NONE',  ( 5.039783919969697656, 28.64334189333860081, -20.38842086786498342 ) ) ;
#10763 = CARTESIAN_POINT ( 'NONE',  ( 43.37500000054622973, 26.92701409722686634, 93.04388485072563242 ) ) ;
#10764 = DIRECTION ( 'NONE',  ( 0.000000000000000000, -0.4999999999999985012, 0.8660254037844394848 ) ) ;
#10765 = ORIENTED_EDGE ( 'NONE', *, *, #1134, .F. ) ;
#10766 = CARTESIAN_POINT ( 'NONE',  ( -4.146808533202904989, 10.89445667252602945, -27.69290272286349364 ) ) ;
#10767 = APPLICATION_PROTOCOL_DEFINITION ( 'draft international standard', 'automotive_design', 1998, #5461 ) ;
#10768 = EDGE_CURVE ( 'NONE', #7687, #7136, #4766, .T. ) ;
#10769 = ADVANCED_FACE ( 'NONE', ( #11595 ), #10634, .T. ) ;
#10770 = CARTESIAN_POINT ( 'NONE',  ( 0.000000000000000000, -2.919948986426525117, 5.057500000000004547 ) ) ;
#10771 = CARTESIAN_POINT ( 'NONE',  ( 49.17500000054622689, 26.19570976099943493, 86.29171490190961435 ) ) ;
#10772 = CARTESIAN_POINT ( 'NONE',  ( 32.07500000054623257, 13.80429023900056507, 95.29460816699764791 ) ) ;
#10773 = CARTESIAN_POINT ( 'NONE',  ( 22.37500000054622262, 12.34168156654572535, 90.79316153445363113 ) ) ;
#10774 = CARTESIAN_POINT ( 'NONE',  ( 25.69999999999998508, 26.37988106264029398, 95.42841645007781892 ) ) ;
#10775 = EDGE_CURVE ( 'NONE', #1359, #10915, #12300, .T. ) ;
#10776 =( LENGTH_UNIT ( ) NAMED_UNIT ( * ) SI_UNIT ( .MILLI., .METRE. ) );
#10777 = CARTESIAN_POINT ( 'NONE',  ( 33.97500000054623115, 15.71886984736413417, 96.68563167572563088 ) ) ;
#10778 = EDGE_LOOP ( 'NONE', ( #12154, #1562, #4929, #8604 ) ) ;
#10779 = CARTESIAN_POINT ( 'NONE',  ( 0.000000000000000000, -5.839897972853060892, 7.806255641895631925E-15 ) ) ;
#10780 = EDGE_LOOP ( 'NONE', ( #11618, #7700 ) ) ;
#10781 = DIRECTION ( 'NONE',  ( 0.000000000000000000, 1.000000000000000000, 0.000000000000000000 ) ) ;
#10782 = ORIENTED_EDGE ( 'NONE', *, *, #2085, .F. ) ;
#10783 = EDGE_CURVE ( 'NONE', #10690, #3966, #8538, .T. ) ;
#10784 = LINE ( 'NONE', #208, #4168 ) ;
#10785 = AXIS2_PLACEMENT_3D ( 'NONE', #6041, #7881, #147 ) ;
#10786 = CARTESIAN_POINT ( 'NONE',  ( 3.061565168526138680E-15, 55.00000000000000000, 25.00000000000000000 ) ) ;
#10787 = CARTESIAN_POINT ( 'NONE',  ( 41.17500000054621978, 26.19570976099943849, 86.29171490190961435 ) ) ;
#10788 = CARTESIAN_POINT ( 'NONE',  ( 39.75000000109247367, 17.56310227825322556, 98.29316153445364534 ) ) ;
#10789 = CARTESIAN_POINT ( 'NONE',  ( 25.99999999999998934, 20.00000000000000355, 98.29316153445363113 ) ) ;
#10790 = CARTESIAN_POINT ( 'NONE',  ( 40.89999999999998437, 17.56310227825321135, 83.29316153445363113 ) ) ;
#10791 = EDGE_CURVE ( 'NONE', #5818, #5150, #3914, .T. ) ;
#10792 = CARTESIAN_POINT ( 'NONE',  ( -9.740943735563897476, 22.28537929251632477, -23.02431258361445288 ) ) ;
#10793 = DIRECTION ( 'NONE',  ( 0.000000000000000000, 0.000000000000000000, -1.000000000000000000 ) ) ;
#10794 = ORIENTED_EDGE ( 'NONE', *, *, #5812, .T. ) ;
#10795 =( REPRESENTATION_RELATIONSHIP ('NONE','NONE', #4262, #8561 ) REPRESENTATION_RELATIONSHIP_WITH_TRANSFORMATION ( #5201 )SHAPE_REPRESENTATION_RELATIONSHIP( ) );
#10796 = VECTOR ( 'NONE', #1015, 1000.000000000000114 ) ;
#10797 = CARTESIAN_POINT ( 'NONE',  ( 29.45000000109246230, 24.40838939219354842, 96.86078899226572503 ) ) ;
#10798 = CARTESIAN_POINT ( 'NONE',  ( 5.000000000000000000, 50.00000000000000000, -24.49489742783178414 ) ) ;
#10799 = ORIENTED_EDGE ( 'NONE', *, *, #8392, .F. ) ;
#10800 = VERTEX_POINT ( 'NONE', #3028 ) ;
#10801 = CARTESIAN_POINT ( 'NONE',  ( 24.85000000109246443, 24.40838939219355197, 84.72553407664153724 ) ) ;
#10802 = FACE_OUTER_BOUND ( 'NONE', #9612, .T. ) ;
#10803 = CARTESIAN_POINT ( 'NONE',  ( 6.000000000000000000, 0.000000000000000000, 0.000000000000000000 ) ) ;
#10804 = CARTESIAN_POINT ( 'NONE',  ( 28.17500000054622689, 13.07298590277314254, 93.04388485072563242 ) ) ;
#10805 = CARTESIAN_POINT ( 'NONE',  ( 33.67500000054622689, 24.28113015263587116, 96.68563167572563088 ) ) ;
#10806 = AXIS2_PLACEMENT_3D ( 'NONE', #10922, #7110, #5157 ) ;
#10807 = DIRECTION ( 'NONE',  ( 1.000000000000000000, 0.000000000000000000, 0.000000000000000000 ) ) ;
#10808 = CARTESIAN_POINT ( 'NONE',  ( 1.321572630236863111, 29.93396655346517576, -27.97622437266944928 ) ) ;
#10809 = CARTESIAN_POINT ( 'NONE',  ( 34.15000000109245804, 12.11403331821300533, 90.79316153445363113 ) ) ;
#10810 = ORIENTED_EDGE ( 'NONE', *, *, #4038, .F. ) ;
#10811 = CARTESIAN_POINT ( 'NONE',  ( 3.055841136373902422, 53.97118948954670969, -24.81406232681816348 ) ) ;
#10812 = DIRECTION ( 'NONE',  ( -0.000000000000000000, -1.000000000000000000, -0.000000000000000000 ) ) ;
#10813 = ORIENTED_EDGE ( 'NONE', *, *, #9696, .F. ) ;
#10814 = LINE ( 'NONE', #300, #7407 ) ;
#10815 = SHAPE_REPRESENTATION ( 'socket head cap screw_iso_ISO 4762 M12 x 80 - 36N', ( #9021 ), #1096 ) ;
#10816 = AXIS2_PLACEMENT_3D ( 'NONE', #7694, #4648, #11561 ) ;
#10817 = VERTEX_POINT ( 'NONE', #10823 ) ;
#10818 = AXIS2_PLACEMENT_3D ( 'NONE', #568, #631, #4374 ) ;
#10819 = DIRECTION ( 'NONE',  ( 0.000000000000000000, 0.000000000000000000, -1.000000000000000000 ) ) ;
#10820 = CARTESIAN_POINT ( 'NONE',  ( -7.514688383768903357, 13.39426057884744026, -23.84485093628785535 ) ) ;
#10821 = CARTESIAN_POINT ( 'NONE',  ( 4.999999999999997335, 0.000000000000000000, 69.99999999999998579 ) ) ;
#10822 = DIRECTION ( 'NONE',  ( 1.000000000000000000, 0.000000000000000000, 0.000000000000000000 ) ) ;
#10823 = CARTESIAN_POINT ( 'NONE',  ( 53.99999999999999289, 20.00000000000000711, 189.0000000000000000 ) ) ;
#10824 = EDGE_CURVE ( 'NONE', #9224, #5074, #6514, .T. ) ;
#10825 = CARTESIAN_POINT ( 'NONE',  ( 0.000000000000000000, 67.00000000000000000, 0.000000000000000000 ) ) ;
#10826 = VECTOR ( 'NONE', #2642, 1000.000000000000000 ) ;
#10827 = FACE_OUTER_BOUND ( 'NONE', #10938, .T. ) ;
#10828 = CARTESIAN_POINT ( 'NONE',  ( 4.839186675186220477, 48.70048224716990148, -20.43493563430346072 ) ) ;
#10829 = CARTESIAN_POINT ( 'NONE',  ( 2.571758278209441661E-15, 139.9999999999999716, 21.00000000000000000 ) ) ;
#10830 = CARTESIAN_POINT ( 'NONE',  ( 40.27500000054623541, 12.34168156654572535, 90.79316153445363113 ) ) ;
#10831 = CARTESIAN_POINT ( 'NONE',  ( -4.744081181139592651, 48.38712208294071360, -24.54608042500704457 ) ) ;
#10832 = VERTEX_POINT ( 'NONE', #5000 ) ;
#10833 = ADVANCED_FACE ( 'NONE', ( #2138 ), #12163, .T. ) ;
#10834 = CARTESIAN_POINT ( 'NONE',  ( 3.549343885166972523, 29.35473140773891032, -24.74867856782190856 ) ) ;
#10835 = ITEM_DEFINED_TRANSFORMATION ( 'NONE', 'NONE', #12231,  #9021 ) ;
#10836 = CIRCLE ( 'NONE', #9834, 0.5999999999999998668 ) ;
#10837 = VECTOR ( 'NONE', #8469, 1000.000000000000000 ) ;
#10838 = B_SPLINE_CURVE_WITH_KNOTS ( 'NONE', 3,
 ( #3684, #11431, #2742, #2163, #5089, #205, #2927, #3112, #9781, #11805, #7812, #3999, #269, #3053, #967, #8005, #9847, #7749, #3938, #1969 ),
 .UNSPECIFIED., .F., .F.,
 ( 4, 2, 2, 2, 2, 2, 2, 2, 2, 4 ),
 ( 0.000000000000000000, 0.0009792184361842109445, 0.001468827654276316742, 0.001958436872368422756, 0.002937655308552634351, 0.003916873744736846380, 0.004896092180921057975, 0.005875310617105269570, 0.006854529053289482032, 0.007833747489473694495 ),
 .UNSPECIFIED. ) ;
#10839 = CARTESIAN_POINT ( 'NONE',  ( 22.37500000054622262, 12.34168156654572357, 90.79316153445363113 ) ) ;
#10840 = CARTESIAN_POINT ( 'NONE',  ( 0.000000000000000000, -2.919948986426525117, 5.057500000000004547 ) ) ;
#10841 = CARTESIAN_POINT ( 'NONE',  ( 33.87500000054621552, 17.63344945572769973, 98.07665518445361386 ) ) ;
#10842 = CARTESIAN_POINT ( 'NONE',  ( 20.17500000054622689, 13.80429023900056507, 95.29460816699764791 ) ) ;
#10843 = CARTESIAN_POINT ( 'NONE',  ( 21.79999999999998650, 24.40838939219354842, 96.86078899226572503 ) ) ;
#10844 = AXIS2_PLACEMENT_3D ( 'NONE', #12227, #3406, #2645 ) ;
#10845 = CARTESIAN_POINT ( 'NONE',  ( 49.09999999999998721, 22.43689772174678509, 83.29316153445363113 ) ) ;
#10846 = CARTESIAN_POINT ( 'NONE',  ( 24.97500000054622760, 24.28113015263587471, 84.90069139318163138 ) ) ;
#10847 = ORIENTED_EDGE ( 'NONE', *, *, #5232, .F. ) ;
#10848 = PRODUCT_DEFINITION_SHAPE ( 'NONE', 'NONE',  #12543 ) ;
#10849 = EDGE_CURVE ( 'NONE', #10504, #9270, #9231, .T. ) ;
#10850 = AXIS2_PLACEMENT_3D ( 'NONE', #8605, #2000, #1812 ) ;
#10851 = DIRECTION ( 'NONE',  ( -0.000000000000000000, -1.000000000000000000, -0.000000000000000000 ) ) ;
#10852 = EDGE_LOOP ( 'NONE', ( #1797, #238, #5786, #7581, #10143 ) ) ;
#10853 = EDGE_LOOP ( 'NONE', ( #8769, #8848, #349, #11060, #9530, #1130 ) ) ;
#10854 = FACE_OUTER_BOUND ( 'NONE', #1633, .T. ) ;
#10855 = ORIENTED_EDGE ( 'NONE', *, *, #8239, .F. ) ;
#10856 = CARTESIAN_POINT ( 'NONE',  ( 0.3301019608631527991, 45.00000000000000711, 28.00000000000000711 ) ) ;
#10857 = CARTESIAN_POINT ( 'NONE',  ( 9.868636702206156741, 18.35145658115177980, -26.20333517057690997 ) ) ;
#10858 = CARTESIAN_POINT ( 'NONE',  ( 38.37500000054622262, 12.34168156654572357, 90.79316153445363113 ) ) ;
#10859 = DIRECTION ( 'NONE',  ( -1.000000000000000000, -0.000000000000000000, -0.000000000000000000 ) ) ;
#10860 = CARTESIAN_POINT ( 'NONE',  ( 26.49999999999998934, 12.11403331821300533, 90.79316153445363113 ) ) ;
#10861 = CARTESIAN_POINT ( 'NONE',  ( 41.27500000054622120, 26.92701409722686634, 88.54243821818162985 ) ) ;
#10862 = CARTESIAN_POINT ( 'NONE',  ( 40.19999999999998863, 15.59161060780645691, 96.86078899226572503 ) ) ;
#10863 = CARTESIAN_POINT ( 'NONE',  ( -8.673894831530475358, 25.01911591053615425, -23.45021177788830968 ) ) ;
#10864 = CARTESIAN_POINT ( 'NONE',  ( 49.77500000054622831, 20.00000000000000355, 98.07665518445361386 ) ) ;
#10865 = VERTEX_POINT ( 'NONE', #2332 ) ;
#10866 = CARTESIAN_POINT ( 'NONE',  ( 29.85000000109246443, 15.59161060780645691, 96.86078899226572503 ) ) ;
#10867 = CARTESIAN_POINT ( 'NONE',  ( -0.3301927727158289749, 10.00000000000000000, 25.00000000000000355 ) ) ;
#10868 = AXIS2_PLACEMENT_3D ( 'NONE', #9508, #6635, #1881 ) ;
#10869 = EDGE_LOOP ( 'NONE', ( #10054, #6330, #7355, #6238, #8697 ) ) ;
#10870 = B_SPLINE_CURVE_WITH_KNOTS ( 'NONE', 3,
 ( #4858, #11581, #10808, #5115, #6880, #4026, #6001, #3140, #6751, #8846, #10744, #3899, #9873, #9683, #993, #8723, #9810, #2056, #38, #5052, #1121, #4089, #7011, #7777 ),
 .UNSPECIFIED., .F., .F.,
 ( 4, 2, 2, 2, 2, 2, 2, 2, 2, 2, 2, 4 ),
 ( 9.545105710734825969E-19, 0.001971105590603967981, 0.002956658385905950020, 0.003942211181207931625, 0.005913316771811892233, 0.006898869567113871670, 0.007884422362415852842, 0.009855527953019816920, 0.01182663354362378100, 0.01281218633892575870, 0.01379773913422773640, 0.01576884472483168140 ),
 .UNSPECIFIED. ) ;
#10871 = DIRECTION ( 'NONE',  ( 1.000000000000000000, 0.000000000000000000, 0.000000000000000000 ) ) ;
#10872 = ORIENTED_EDGE ( 'NONE', *, *, #7862, .T. ) ;
#10873 = CARTESIAN_POINT ( 'NONE',  ( -2.000000000000015543, 20.00000000000000355, 98.29316153445363113 ) ) ;
#10874 = EDGE_CURVE ( 'NONE', #9164, #11587, #3262, .T. ) ;
#10875 = DIRECTION ( 'NONE',  ( -1.000000000000000000, -0.000000000000000000, -0.000000000000000000 ) ) ;
#10876 = DIRECTION ( 'NONE',  ( -1.000000000000000000, -0.000000000000000000, -0.000000000000000000 ) ) ;
#10877 = VECTOR ( 'NONE', #50, 1000.000000000000000 ) ;
#10878 = CARTESIAN_POINT ( 'NONE',  ( 32.57500000054623257, 15.71886984736413773, 84.90069139318163138 ) ) ;
#10879 = CARTESIAN_POINT ( 'NONE',  ( 31.27500000054622831, 26.92701409722686634, 88.54243821818162985 ) ) ;
#10880 =( REPRESENTATION_RELATIONSHIP ('NONE','NONE', #4262, #10013 ) REPRESENTATION_RELATIONSHIP_WITH_TRANSFORMATION ( #3412 )SHAPE_REPRESENTATION_RELATIONSHIP( ) );
#10881 = DIRECTION ( 'NONE',  ( -0.000000000000000000, -1.000000000000000000, -0.000000000000000000 ) ) ;
#10882 = EDGE_CURVE ( 'NONE', #7598, #1223, #10836, .T. ) ;
#10883 = DIRECTION ( 'NONE',  ( 0.000000000000000000, 0.000000000000000000, -1.000000000000000000 ) ) ;
#10884 = DIRECTION ( 'NONE',  ( 0.000000000000000000, 0.000000000000000000, -1.000000000000000000 ) ) ;
#10885 = ORIENTED_EDGE ( 'NONE', *, *, #7535, .F. ) ;
#10886 = DIRECTION ( 'NONE',  ( -0.000000000000000000, 1.000000000000000000, 1.224646799147353207E-16 ) ) ;
#10887 = DIRECTION ( 'NONE',  ( 1.000000000000000000, 0.000000000000000000, 0.000000000000000000 ) ) ;
#10888 = VERTEX_POINT ( 'NONE', #7208 ) ;
#10889 = DIRECTION ( 'NONE',  ( -1.000000000000000000, 0.000000000000000000, 0.000000000000000000 ) ) ;
#10890 = ORIENTED_EDGE ( 'NONE', *, *, #11189, .T. ) ;
#10891 = VECTOR ( 'NONE', #9292, 1000.000000000000000 ) ;
#10892 = CARTESIAN_POINT ( 'NONE',  ( -7.929079634139357680, 13.89786668772332767, -23.71027527960010417 ) ) ;
#10893 = DIRECTION ( 'NONE',  ( -0.000000000000000000, -1.000000000000000000, -0.000000000000000000 ) ) ;
#10894 = DIRECTION ( 'NONE',  ( 0.000000000000000000, -0.5000000000000012212, -0.8660254037844380415 ) ) ;
#10895 = CIRCLE ( 'NONE', #12504, 7.499999999999978684 ) ;
#10896 = CARTESIAN_POINT ( 'NONE',  ( 9.989996519715994339, 20.51596962592459406, 98.27983912618213935 ) ) ;
#10897 = CARTESIAN_POINT ( 'NONE',  ( 3.975724277407679974, 46.95046481276702366, -24.68253032026751370 ) ) ;
#10898 = DIRECTION ( 'NONE',  ( 0.000000000000000000, -1.000000000000000000, -0.000000000000000000 ) ) ;
#10899 = DIRECTION ( 'NONE',  ( 1.000000000000000000, -0.000000000000000000, -0.000000000000000000 ) ) ;
#10900 = CARTESIAN_POINT ( 'NONE',  ( -4.247064150047941133, 47.35626993272530427, 27.67617995880919324 ) ) ;
#10901 = CARTESIAN_POINT ( 'NONE',  ( 41.77500000054622831, 20.00000000000000355, 98.07665518445361386 ) ) ;
#10902 = LINE ( 'NONE', #12229, #10962 ) ;
#10903 = ORIENTED_EDGE ( 'NONE', *, *, #11423, .T. ) ;
#10904 = AXIS2_PLACEMENT_3D ( 'NONE', #6553, #3633, #8344 ) ;
#10905 = LINE ( 'NONE', #8914, #11109 ) ;
#10906 = EDGE_CURVE ( 'NONE', #9150, #3211, #11861, .T. ) ;
#10907 = CARTESIAN_POINT ( 'NONE',  ( 21.27500000054622475, 26.92701409722686634, 88.54243821818162985 ) ) ;
#10908 = CARTESIAN_POINT ( 'NONE',  ( 45.67500000054621978, 24.28113015263587116, 96.68563167572563088 ) ) ;
#10909 = CARTESIAN_POINT ( 'NONE',  ( 34.87500000054622973, 22.36655054427230382, 83.50966788445364841 ) ) ;
#10910 = AXIS2_PLACEMENT_3D ( 'NONE', #119, #5001, #3977 ) ;
#10911 = CARTESIAN_POINT ( 'NONE',  ( 24.37500000054622262, 12.34168156654572535, 90.79316153445363113 ) ) ;
#10912 = CARTESIAN_POINT ( 'NONE',  ( 23.49999999999998934, 27.88596668178699645, 90.79316153445363113 ) ) ;
#10913 = DIRECTION ( 'NONE',  ( -0.000000000000000000, -0.000000000000000000, 1.000000000000000000 ) ) ;
#10914 = CARTESIAN_POINT ( 'NONE',  ( 29.37500000054622973, 26.92701409722686634, 93.04388485072563242 ) ) ;
#10915 = VERTEX_POINT ( 'NONE', #8355 ) ;
#10916 = CARTESIAN_POINT ( 'NONE',  ( 22.75000000109246656, 22.43689772174679575, 83.29316153445363113 ) ) ;
#10917 = ORIENTED_EDGE ( 'NONE', *, *, #7705, .F. ) ;
#10918 = ORIENTED_EDGE ( 'NONE', *, *, #8153, .T. ) ;
#10919 = FACE_OUTER_BOUND ( 'NONE', #1970, .T. ) ;
#10920 = EDGE_LOOP ( 'NONE', ( #929, #10039, #7748, #3050, #5863 ) ) ;
#10921 = EDGE_CURVE ( 'NONE', #8859, #9622, #6388, .T. ) ;
#10922 = CARTESIAN_POINT ( 'NONE',  ( 0.000000000000000000, 0.000000000000000000, 0.000000000000000000 ) ) ;
#10923 = AXIS2_PLACEMENT_3D ( 'NONE', #12059, #10325, #11160 ) ;
#10924 = DIRECTION ( 'NONE',  ( -1.000000000000000000, 0.000000000000000000, -0.000000000000000000 ) ) ;
#10925 = CARTESIAN_POINT ( 'NONE',  ( 39.47500000054622404, 26.92701409722686634, 93.04388485072563242 ) ) ;
#10926 = DIRECTION ( 'NONE',  ( 1.000000000000000000, 0.000000000000000000, 0.000000000000000000 ) ) ;
#10927 = EDGE_CURVE ( 'NONE', #10300, #9486, #2573, .T. ) ;
#10928 = CARTESIAN_POINT ( 'NONE',  ( 38.57500000054622546, 13.80429023900056684, 86.29171490190961435 ) ) ;
#10929 = CARTESIAN_POINT ( 'NONE',  ( 42.09999999999997300, 17.56310227825320425, 98.29316153445363113 ) ) ;
#10930 = CARTESIAN_POINT ( 'NONE',  ( 48.17500000054623399, 13.07298590277314254, 93.04388485072563242 ) ) ;
#10931 = VECTOR ( 'NONE', #3791, 1000.000000000000000 ) ;
#10932 = ORIENTED_EDGE ( 'NONE', *, *, #4994, .T. ) ;
#10933 = CARTESIAN_POINT ( 'NONE',  ( 23.75000000109246301, 17.56310227825320425, 98.29316153445363113 ) ) ;
#10934 = CARTESIAN_POINT ( 'NONE',  ( 6.000000000000000000, 4.379923479639802331, 2.528749999999995168 ) ) ;
#10935 = VERTEX_POINT ( 'NONE', #616 ) ;
#10936 = AXIS2_PLACEMENT_3D ( 'NONE', #12142, #12081, #9228 ) ;
#10937 = CARTESIAN_POINT ( 'NONE',  ( 23.09999999999998721, 22.43689772174679575, 83.29316153445363113 ) ) ;
#10938 = EDGE_LOOP ( 'NONE', ( #9238, #11526, #6302, #4831, #3513 ) ) ;
#10939 = DIRECTION ( 'NONE',  ( 1.000000000000000000, -0.000000000000000000, -0.000000000000000000 ) ) ;
#10940 = DIRECTION ( 'NONE',  ( -0.000000000000000000, -0.000000000000000000, -1.000000000000000000 ) ) ;
#10941 = CARTESIAN_POINT ( 'NONE',  ( 48.99999999999998579, 20.00000000000000355, 83.29316153445364534 ) ) ;
#10942 = PRODUCT_DEFINITION_CONTEXT ( 'detailed design', #8857, 'design' ) ;
#10943 = CARTESIAN_POINT ( 'NONE',  ( 28.87500000054622262, 22.36655054427230382, 83.50966788445364841 ) ) ;
#10944 = CARTESIAN_POINT ( 'NONE',  ( 31.57500000054622191, 26.19570976099943493, 95.29460816699764791 ) ) ;
#10945 = B_SPLINE_CURVE_WITH_KNOTS ( 'NONE', 3,
 ( #6084, #11917, #3224, #2972, #5892, #9890, #5196, #4042, #3160, #7025, #7086, #10967, #2212, #2141, #9064, #3091, #3918, #2275, #6142, #10017 ),
 .UNSPECIFIED., .F., .F.,
 ( 4, 2, 2, 2, 2, 2, 2, 2, 2, 4 ),
 ( 0.01568868358392457724, 0.01666917987226885015, 0.01764967616061312305, 0.01863017244895739596, 0.01961066873730166887, 0.02059116502564593831, 0.02157166131399021469, 0.02255215760233448760, 0.02304240574650662232, 0.02353265389067876051 ),
 .UNSPECIFIED. ) ;
#10946 = CARTESIAN_POINT ( 'NONE',  ( 9.740751885065668247, 22.28587776697542466, 26.25114245506233601 ) ) ;
#10947 = DIRECTION ( 'NONE',  ( 0.000000000000000000, -1.000000000000000000, 1.110768649713241713E-15 ) ) ;
#10948 = CARTESIAN_POINT ( 'NONE',  ( -1.300905012451813336, 45.16112489716824996, 24.96819491493427634 ) ) ;
#10949 = ORIENTED_EDGE ( 'NONE', *, *, #12401, .F. ) ;
#10950 = EDGE_CURVE ( 'NONE', #7418, #4704, #1268, .T. ) ;
#10951 = FACE_OUTER_BOUND ( 'NONE', #5618, .T. ) ;
#10952 = DIRECTION ( 'NONE',  ( 0.000000000000000000, -0.4999999999999985012, 0.8660254037844394848 ) ) ;
#10953 = ORIENTED_EDGE ( 'NONE', *, *, #9329, .F. ) ;
#10954 = PLANE ( 'NONE',  #3764 ) ;
#10955 = AXIS2_PLACEMENT_3D ( 'NONE', #10672, #92, #2878 ) ;
#10956 = EDGE_LOOP ( 'NONE', ( #10885, #9938, #11258 ) ) ;
#10957 = CARTESIAN_POINT ( 'NONE',  ( -9.673467176944807733, 17.38163042592174889, -23.05306748635229752 ) ) ;
#10958 = EDGE_CURVE ( 'NONE', #5355, #2550, #6787, .T. ) ;
#10959 = ADVANCED_FACE ( 'NONE', ( #4667 ), #3704, .F. ) ;
#10960 = ADVANCED_FACE ( 'NONE', ( #735 ), #3586, .T. ) ;
#10961 = CARTESIAN_POINT ( 'NONE',  ( -34.99999999999999289, 20.00000000000000355, 170.0000119999999697 ) ) ;
#10962 = VECTOR ( 'NONE', #4676, 999.9999999999998863 ) ;
#10963 = PRODUCT ( 'Bearing', 'Bearing', '', ( #953 ) ) ;
#10964 = CARTESIAN_POINT ( 'NONE',  ( 7.421492300118300633, 26.70405649111976842, 87.42232753731605044 ) ) ;
#10965 = CARTESIAN_POINT ( 'NONE',  ( -31.74999999999995737, 7.347880794884118750E-16, -5.999999999999999112 ) ) ;
#10966 = CARTESIAN_POINT ( 'NONE',  ( 7.942924499382692183, 26.10933434278762988, 19.44382864746247819 ) ) ;
#10967 = CARTESIAN_POINT ( 'NONE',  ( -2.509638519179916205, 54.33675374340515418, 20.85128429580866083 ) ) ;
#10968 = CARTESIAN_POINT ( 'NONE',  ( 4.166436715168401861, 29.09658851243931821, -20.58482738948554314 ) ) ;
#10969 = CARTESIAN_POINT ( 'NONE',  ( 42.17500000054622689, 13.07298590277314254, 93.04388485072563242 ) ) ;
#10970 = CARTESIAN_POINT ( 'NONE',  ( 2.571758291765529985E-15, 45.00000000000000711, 21.00000000000000000 ) ) ;
#10971 = ORIENTED_EDGE ( 'NONE', *, *, #391, .F. ) ;
#10972 = CIRCLE ( 'NONE', #9757, 5.057500000000000107 ) ;
#10973 = CARTESIAN_POINT ( 'NONE',  ( -2.508190414677843982, 54.33763061856527088, 24.87535316732256163 ) ) ;
#10974 = CARTESIAN_POINT ( 'NONE',  ( 20.07500000054622546, 15.71886984736413417, 96.68563167572563088 ) ) ;
#10975 = CARTESIAN_POINT ( 'NONE',  ( 46.47500000054622404, 13.07298590277314432, 88.54243821818161564 ) ) ;
#10976 = CARTESIAN_POINT ( 'NONE',  ( 34.17500000054622689, 13.07298590277314254, 93.04388485072563242 ) ) ;
#10977 = CARTESIAN_POINT ( 'NONE',  ( 23.67500000054622333, 24.28113015263587116, 96.68563167572563088 ) ) ;
#10978 = FACE_OUTER_BOUND ( 'NONE', #11891, .T. ) ;
#10979 = FACE_OUTER_BOUND ( 'NONE', #455, .T. ) ;
#10980 = CARTESIAN_POINT ( 'NONE',  ( 24.07500000054622902, 13.80429023900056507, 95.29460816699764791 ) ) ;
#10981 = ORIENTED_EDGE ( 'NONE', *, *, #482, .F. ) ;
#10982 = CYLINDRICAL_SURFACE ( 'NONE', #10145, 6.000000000000000000 ) ;
#10983 = VERTEX_POINT ( 'NONE', #5749 ) ;
#10984 = EDGE_LOOP ( 'NONE', ( #5879, #6035, #10736, #5007, #2096 ) ) ;
#10985 = CARTESIAN_POINT ( 'NONE',  ( 6.000000000000000000, 2.919948986426538884, 5.057499999999996554 ) ) ;
#10986 = VERTEX_POINT ( 'NONE', #7525 ) ;
#10987 = DIRECTION ( 'NONE',  ( 0.000000000000000000, 0.000000000000000000, 1.000000000000000000 ) ) ;
#10988 = CARTESIAN_POINT ( 'NONE',  ( 37.77500000054622120, 22.36655054427230027, 98.07665518445361386 ) ) ;
#10989 = CARTESIAN_POINT ( 'NONE',  ( 6.000000000000000000, 5.839897972853064445, -8.673617379884035472E-15 ) ) ;
#10990 = CARTESIAN_POINT ( 'NONE',  ( -4.871678679536868728, 48.86275246128555239, -27.57295404460982269 ) ) ;
#10991 = CARTESIAN_POINT ( 'NONE',  ( 37.89999999999999147, 22.43689772174679575, 98.29316153445363113 ) ) ;
#10992 = EDGE_CURVE ( 'NONE', #5152, #8715, #11514, .T. ) ;
#10993 = CARTESIAN_POINT ( 'NONE',  ( 47.97500000054622404, 15.71886984736413417, 96.68563167572563088 ) ) ;
#10994 = ORIENTED_EDGE ( 'NONE', *, *, #12401, .T. ) ;
#10995 = CARTESIAN_POINT ( 'NONE',  ( 25.65000000109246514, 20.00000000000000355, 98.29316153445363113 ) ) ;
#10996 = CARTESIAN_POINT ( 'NONE',  ( -2.645619823791141467, 45.75416279094086036, 24.85999165416970413 ) ) ;
#10997 = ORIENTED_EDGE ( 'NONE', *, *, #4951, .T. ) ;
#10998 = CARTESIAN_POINT ( 'NONE',  ( 5.000000000000000000, 4.685197434473814759, -5.637851296924623057E-15 ) ) ;
#10999 = ORIENTED_EDGE ( 'NONE', *, *, #1755, .T. ) ;
#11000 = CARTESIAN_POINT ( 'NONE',  ( 24.95000000109246585, 26.37988106264029398, 86.15790661882942914 ) ) ;
#11001 = DIRECTION ( 'NONE',  ( -0.000000000000000000, -0.000000000000000000, 1.000000000000000000 ) ) ;
#11002 = CARTESIAN_POINT ( 'NONE',  ( 25.09999999999998366, 22.43689772174679575, 83.29316153445363113 ) ) ;
#11003 = CARTESIAN_POINT ( 'NONE',  ( 31.37500000054622973, 26.92701409722686634, 93.04388485072563242 ) ) ;
#11004 = CARTESIAN_POINT ( 'NONE',  ( 31.87500000054622262, 20.00000000000000355, 98.07665518445361386 ) ) ;
#11005 = VECTOR ( 'NONE', #12057, 1000.000000000000000 ) ;
#11006 = CARTESIAN_POINT ( 'NONE',  ( 8.977351811841533191, 24.45372485761732761, 26.52316716509305294 ) ) ;
#11007 = CARTESIAN_POINT ( 'NONE',  ( 49.99999999999998579, 0.000000000000000000, 82.99999999999995737 ) ) ;
#11008 = ORIENTED_EDGE ( 'NONE', *, *, #9208, .T. ) ;
#11009 = CARTESIAN_POINT ( 'NONE',  ( 46.05000000109246372, 12.86707612778636012, 93.11078899226572503 ) ) ;
#11010 =( LENGTH_UNIT ( ) NAMED_UNIT ( * ) SI_UNIT ( .MILLI., .METRE. ) );
#11011 = EDGE_LOOP ( 'NONE', ( #2900, #6037, #11872, #11103, #8394, #9243, #4215, #6381, #1374, #4753, #6645, #1282, #10718 ) ) ;
#11012 = CARTESIAN_POINT ( 'NONE',  ( -50.00000000000001421, 22.00000000000000000, 188.4007504869563263 ) ) ;
#11013 = ADVANCED_FACE ( 'NONE', ( #3770 ), #9620, .F. ) ;
#11014 = ORIENTED_EDGE ( 'NONE', *, *, #1196, .T. ) ;
#11015 = CARTESIAN_POINT ( 'NONE',  ( -1.314141907159803946, 10.08123752450589095, -24.96759818712484957 ) ) ;
#11016 = AXIS2_PLACEMENT_3D ( 'NONE', #7718, #10621, #7464 ) ;
#11017 = CARTESIAN_POINT ( 'NONE',  ( 4.452539714567801177, 11.03997247681473404, -24.60205477162727661 ) ) ;
#11018 = AXIS2_PLACEMENT_3D ( 'NONE', #884, #9522, #4755 ) ;
#11019 = CARTESIAN_POINT ( 'NONE',  ( -10.00000000000000355, 20.00000000000000355, -28.00000000000000711 ) ) ;
#11020 =( NAMED_UNIT ( * ) PLANE_ANGLE_UNIT ( ) SI_UNIT ( $, .RADIAN. ) );
#11021 = CARTESIAN_POINT ( 'NONE',  ( 38.35000000109246798, 13.62011893735970958, 86.15790661882942914 ) ) ;
#11022 = CARTESIAN_POINT ( 'NONE',  ( 92.00000000000000000, 5.035999999999999588, 0.000000000000000000 ) ) ;
#11023 = DIRECTION ( 'NONE',  ( 1.000000000000000000, 0.000000000000000000, 0.000000000000000000 ) ) ;
#11024 = FACE_OUTER_BOUND ( 'NONE', #7367, .T. ) ;
#11025 = CARTESIAN_POINT ( 'NONE',  ( -1.137267047700306843, 45.12832572938893350, 27.97735201090558732 ) ) ;
#11026 = VECTOR ( 'NONE', #2499, 1000.000000000000000 ) ;
#11027 = EDGE_CURVE ( 'NONE', #3844, #12462, #11247, .T. ) ;
#11028 = CARTESIAN_POINT ( 'NONE',  ( -4.555463605440090546, 47.93247208080379806, -24.58153461361902359 ) ) ;
#11029 = ORIENTED_EDGE ( 'NONE', *, *, #1496, .T. ) ;
#11030 = LINE ( 'NONE', #8116, #11310 ) ;
#11031 = ADVANCED_FACE ( 'NONE', ( #7588 ), #1924, .T. ) ;
#11032 = CIRCLE ( 'NONE', #6382, 0.5999999999999998668 ) ;
#11033 = CARTESIAN_POINT ( 'NONE',  ( 28.69999999999998508, 13.62011893735970958, 86.15790661882942914 ) ) ;
#11034 = CARTESIAN_POINT ( 'NONE',  ( 44.97500000054621694, 22.36655054427230382, 83.50966788445364841 ) ) ;
#11035 = CARTESIAN_POINT ( 'NONE',  ( 27.67500000054622689, 22.36655054427230027, 98.07665518445361386 ) ) ;
#11036 =( BOUNDED_CURVE ( )  B_SPLINE_CURVE ( 2, ( #2793, #4696, #827, #1837, #12499, #12379, #9466, #2920, #8569, #6655, #12440 ),
 .UNSPECIFIED., .F., .F. ) 
 B_SPLINE_CURVE_WITH_KNOTS ( ( 3, 2, 2, 2, 2, 3 ),
 ( 0.6333333333333333037, 0.6400000000000000133, 0.6466666666666666119, 0.6533333333333333215, 0.6600000000000000311, 0.6666666666666666297 ),
 .UNSPECIFIED. ) 
 CURVE ( )  GEOMETRIC_REPRESENTATION_ITEM ( )  RATIONAL_B_SPLINE_CURVE ( ( 1.000000000000000000, 0.9510565162951535312, 1.000000000000000000, 0.9510565162951535312, 1.000000000000000000, 0.9510565162951535312, 1.000000000000000000, 0.9510565162951535312, 1.000000000000000000, 0.9510565162951535312, 1.000000000000000000 ) ) 
 REPRESENTATION_ITEM ( '' )  );
#11037 = CARTESIAN_POINT ( 'NONE',  ( 10.00000000000000178, 19.47976500067654726, 83.29316153445364534 ) ) ;
#11038 = DIRECTION ( 'NONE',  ( 1.000000000000000000, 0.000000000000000000, 0.000000000000000000 ) ) ;
#11039 = CARTESIAN_POINT ( 'NONE',  ( -36.00000000000000711, 72.60660171779821326, 154.3533255156881694 ) ) ;
#11041 = ADVANCED_FACE ( 'NONE', ( #2700 ), #4361, .T. ) ;
#11040 = CARTESIAN_POINT ( 'NONE',  ( 23.57500000054622902, 24.28113015263587116, 96.68563167572563088 ) ) ;
#11042 = ORIENTED_EDGE ( 'NONE', *, *, #4832, .T. ) ;
#11043 = CARTESIAN_POINT ( 'NONE',  ( 32.65000000109246514, 20.00000000000000355, 83.29316153445364534 ) ) ;
#11044 = ORIENTED_EDGE ( 'NONE', *, *, #3804, .F. ) ;
#11045 = DIRECTION ( 'NONE',  ( 0.000000000000000000, 0.000000000000000000, -1.000000000000000000 ) ) ;
#11046 = AXIS2_PLACEMENT_3D ( 'NONE', #5858, #1974, #2871 ) ;
#11047 = VERTEX_POINT ( 'NONE', #8597 ) ;
#11048 = CIRCLE ( 'NONE', #5579, 7.500000000000000000 ) ;
#11049 = APPLICATION_CONTEXT ( 'automotive_design' ) ;
#11050 = CARTESIAN_POINT ( 'NONE',  ( 33.07500000054622546, 24.28113015263587471, 84.90069139318163138 ) ) ;
#11051 = LINE ( 'NONE', #5282, #10378 ) ;
#11052 = CARTESIAN_POINT ( 'NONE',  ( 20.35000000109246088, 13.62011893735970958, 86.15790661882942914 ) ) ;
#11053 = CARTESIAN_POINT ( 'NONE',  ( 31.77500000054622475, 22.36655054427230027, 98.07665518445361386 ) ) ;
#11054 = EDGE_CURVE ( 'NONE', #7325, #1799, #799, .T. ) ;
#11055 = CARTESIAN_POINT ( 'NONE',  ( 37.99999999999999289, 20.00000000000000355, 98.29316153445363113 ) ) ;
#11056 = CARTESIAN_POINT ( 'NONE',  ( 46.47500000054623115, 13.80429023900056684, 86.29171490190961435 ) ) ;
#11057 = ORIENTED_EDGE ( 'NONE', *, *, #12180, .F. ) ;
#11058 = CARTESIAN_POINT ( 'NONE',  ( 27.35000000109246798, 26.37988106264029398, 95.42841645007781892 ) ) ;
#11059 = CARTESIAN_POINT ( 'NONE',  ( -3.974987698915826595, 46.94954269600466290, 24.68264807992340337 ) ) ;
#11060 = ORIENTED_EDGE ( 'NONE', *, *, #2173, .F. ) ;
#11061 = DIRECTION ( 'NONE',  ( 1.000000000000000000, 0.000000000000000000, 0.000000000000000000 ) ) ;
#11062 = AXIS2_PLACEMENT_3D ( 'NONE', #10700, #5894, #9516 ) ;
#11063 = ORIENTED_EDGE ( 'NONE', *, *, #4489, .F. ) ;
#11064 = CARTESIAN_POINT ( 'NONE',  ( 9.357362328184084532, 16.45777577070792219, 26.39048341541894871 ) ) ;
#11065 = CARTESIAN_POINT ( 'NONE',  ( 4.484841213128739845, 47.78346385583337508, -27.63860224454065317 ) ) ;
#11066 = EDGE_CURVE ( 'NONE', #9719, #918, #9031, .T. ) ;
#11067 = CARTESIAN_POINT ( 'NONE',  ( -2.000000000000015543, 20.00000000000000355, 98.29316153445363113 ) ) ;
#11068 = CARTESIAN_POINT ( 'NONE',  ( 31.67500000054622689, 22.36655054427230027, 98.07665518445361386 ) ) ;
#11069 = CARTESIAN_POINT ( 'NONE',  ( 24.27500000054622475, 13.07298590277314254, 93.04388485072563242 ) ) ;
#11070 = DIRECTION ( 'NONE',  ( 0.000000000000000000, 0.000000000000000000, -1.000000000000000000 ) ) ;
#11071 = CARTESIAN_POINT ( 'NONE',  ( -1.002883791299520887E-19, 10.00000000000000000, -25.00000000000000000 ) ) ;
#11072 = EDGE_LOOP ( 'NONE', ( #6188, #6700, #43 ) ) ;
#11073 = CARTESIAN_POINT ( 'NONE',  ( 46.45000000109246230, 15.59161060780646046, 84.72553407664153724 ) ) ;
#11074 = ORIENTED_EDGE ( 'NONE', *, *, #868, .F. ) ;
#11075 = DIRECTION ( 'NONE',  ( 0.000000000000000000, -0.5000000000000011102, -0.8660254037844379305 ) ) ;
#11076 = ORIENTED_EDGE ( 'NONE', *, *, #1568, .F. ) ;
#11077 = CARTESIAN_POINT ( 'NONE',  ( -5.024407006007729493, 11.34777053809138003, -20.39219789878416478 ) ) ;
#11078 = AXIS2_PLACEMENT_3D ( 'NONE', #3974, #3282, #4167 ) ;
#11079 = CARTESIAN_POINT ( 'NONE',  ( -6.608338170980154302, 27.53359326989389189, 24.11557641055247458 ) ) ;
#11080 = DIRECTION ( 'NONE',  ( 0.000000000000000000, -0.5000000000000014433, -0.8660254037844379305 ) ) ;
#11081 = CARTESIAN_POINT ( 'NONE',  ( 4.337826254667723092, 52.50833866356535395, 24.62149076657007640 ) ) ;
#11082 = EDGE_CURVE ( 'NONE', #2709, #9039, #9496, .T. ) ;
#11083 = CARTESIAN_POINT ( 'NONE',  ( -2.618974170005213153, 10.32668121623932400, 24.87084347637328108 ) ) ;
#11084 = CARTESIAN_POINT ( 'NONE',  ( 0.000000000000000000, 22.00000000000000000, 169.9999999999999716 ) ) ;
#11085 = DIRECTION ( 'NONE',  ( -0.000000000000000000, -1.000000000000000000, -0.000000000000000000 ) ) ;
#11086 = CYLINDRICAL_SURFACE ( 'NONE', #876, 7.500000000000007105 ) ;
#11087 = CARTESIAN_POINT ( 'NONE',  ( 8.664233696039474353, 25.03468766560890302, 23.45371044974007901 ) ) ;
#11088 = CARTESIAN_POINT ( 'NONE',  ( 4.491162728695237583, 47.77810914732295799, 20.51453334527777628 ) ) ;
#11089 = EDGE_LOOP ( 'NONE', ( #5788, #1077, #8820 ) ) ;
#11090 = CARTESIAN_POINT ( 'NONE',  ( -4.839306774598123084, 51.30008082132634684, 24.52723862394605092 ) ) ;
#11091 = CARTESIAN_POINT ( 'NONE',  ( 2.216120825188211185, 45.50613141711284015, 24.90340997055814398 ) ) ;
#11092 = VECTOR ( 'NONE', #7348, 1000.000000000000000 ) ;
#11093 = CARTESIAN_POINT ( 'NONE',  ( 10.00000000000000355, 20.00000000000000355, -66.99999999999998579 ) ) ;
#11094 = CARTESIAN_POINT ( 'NONE',  ( 45.97500000054623115, 17.63344945572769973, 98.07665518445361386 ) ) ;
#11095 = CARTESIAN_POINT ( 'NONE',  ( 24.47500000054623115, 13.80429023900056684, 86.29171490190961435 ) ) ;
#11096 = CARTESIAN_POINT ( 'NONE',  ( 6.843016236096653770, 12.70761845378527610, 92.56370047283017755 ) ) ;
#11097 = CARTESIAN_POINT ( 'NONE',  ( 45.55000000109246372, 22.43689772174676023, 98.29316153445364534 ) ) ;
#11098 = DIRECTION ( 'NONE',  ( 0.000000000000000000, 0.000000000000000000, -1.000000000000000000 ) ) ;
#11099 = CARTESIAN_POINT ( 'NONE',  ( -2.000000000000015543, 20.00000000000000355, 90.79316153445363113 ) ) ;
#11100 = ORIENTED_EDGE ( 'NONE', *, *, #640, .F. ) ;
#11101 = EDGE_CURVE ( 'NONE', #5431, #169, #10047, .T. ) ;
#11102 = CARTESIAN_POINT ( 'NONE',  ( 34.99999999999998579, 20.00000000000000000, 137.5000000000000000 ) ) ;
#11103 = ORIENTED_EDGE ( 'NONE', *, *, #1089, .F. ) ;
#11104 = CARTESIAN_POINT ( 'NONE',  ( 0.000000000000000000, 20.00000000000000355, 69.99999999999998579 ) ) ;
#11105 = ORIENTED_EDGE ( 'NONE', *, *, #4562, .T. ) ;
#11106 = EDGE_CURVE ( 'NONE', #4145, #667, #4728, .T. ) ;
#11108 = EDGE_CURVE ( 'NONE', #5910, #7043, #3342, .T. ) ;
#11107 =( BOUNDED_SURFACE ( )  B_SPLINE_SURFACE ( 1, 2, ( 
 ( #1213, #2020, #6846, #3928, #10709, #1025, #4885, #10771, #4115, #8747, #7803, #11675, #5902, #9771, #5079, #7866, #2084, #7740, #2852, #6715, #10582, #9648, #956, #2915, #8059, #2223, #8245, #5204, #5328, #1271, #5142, #10027, #2344, #1336, #10975, #3233, #4247, #2283, #6152, #11094, #4305, #8182, #10908, #9074, #11988, #7994, #12054, #443, #11863, #11034, #6092, #382, #12114, #2460, #9964, #3416, #9198, #8119, #9010, #7285, #6276, #6212, #6336, #321, #3293, #7156, #10086, #10203, #508, #1398, #5265, #9137, #3170, #3354, #7222, #4183, #1515, #5392, #11926, #4370, #7094, #7034, #2400, #10148, #1460, #11155, #9263, #564, #5872, #11645, #8489, #1753, #1991, #7774, #7344, #10382, #1578, #6517, #5517, #1695, #3538, #12175, #9510, #10261, #2952, #5456, #1637, #8307, #11214, #12361, #10320, #3661, #4427, #687, #9447, #3897, #6817, #9325, #2526, #10680, #12298, #7537, #6579, #11280, #4615, #7411, #9744, #5576, #2587, #4492, #9385, #749, #4554, #11404, #3478, #4857, #2714, #6397, #627, #8366, #8428, #991, #6459, #3598, #12235, #7474, #11348, #10443, #2654, #8722, #5637, #35, #10743, #4023, #3962, #5177, #8093, #3205, #5934, #6126, #230, #2257, #10805, #7009, #3268, #6061, #7838, #7130, #11768, #9994, #11707, #11959, #1307, #2121, #4087, #5998, #8782, #5113, #9871, #2054, #11004, #2316, #1118, #10944, #8845, #1058, #10879, #102, #7962, #3011, #1184, #9807, #6185, #4920, #8977, #9046, #6879, #4221, #4984, #2190, #165, #3138, #5050, #9934, #7898, #3074, #357, #6937, #8911, #11830, #1242, #291, #4154, #8029, #11900, #7067, #10060, #6313, #2497, #9360, #4525, #2376, #8155, #3570, #5363, #601, #12208, #4343, #10239, #477, #12272, #11191, #8217, #10123, #7255, #6372, #11129, #1552, #11316, #10293, #5425, #1371, #9109, #660, #10179, #6431, #12086, #9170, #1434, #1487, #538, #3455, #7192, #1611, #6245, #2435, #11069, #3388, #416, #5491, #8401, #3509, #5301, #2557, #9234, #11250, #4401, #7319, #7446, #9296, #4277, #2623, #8278, #5237, #12021, #12147, #4463, #3325, #8342, #7380, #10354, #9546, #4589, #12393, #10598, #977, #9420, #1912, #3821, #11439, #8462, #5797, #4780, #4712, #4842, #12331, #10480, #6609, #844, #10543, #7697 ),
 ( #1669, #11564, #3631, #8709, #7508, #3692, #5551, #722, #1853, #7571, #5735, #6491, #2749, #11501, #9667, #21, #11380, #2685, #3883, #1789, #9601, #8645, #782, #6673, #9482, #7757, #7635, #4651, #6550, #5675, #2809, #8583, #911, #11629, #6734, #12517, #10417, #1731, #5610, #12454, #2873, #8521, #3756, #6865, #11753, #5981, #8897, #84, #3190, #7824, #4007, #3947, #5921, #5860, #7051, #9981, #5098, #11690, #8012, #2104, #4139, #150, #215, #5163, #7950, #9729, #9030, #1102, #11885, #1046, #4968, #6924, #2934, #6991, #11815, #6800, #9855, #4907, #8831, #10929, #1290, #8766, #2243, #276, #7884, #2998, #6110, #1228, #1170, #342, #10728, #10790, #3062, #5033, #4205, #8079, #4072, #3122, #10862, #10666, #2172, #6045, #2041, #1976, #9791, #9919, #8963, #7177, #11946, #9217, #7117, #2419, #6170, #9156, #8141, #645, #6414, #1473, #462, #5346, #11055, #10991, #4449, #5223, #10277, #9094, #4324, #3251, #2301, #3439, #5285, #11176, #10046, #8201, #4384, #11232, #1595, #4264, #1357, #5476, #7241, #2479, #1535, #6232, #12131, #2362, #9342, #523, #10105, #12007, #12071, #8261, #3372, #7301, #4508, #12192, #6354, #401, #3309, #2542, #11114, #8326, #1418, #6296, #10167, #10222, #5408, #9279, #583, #3493, #7364, #9465, #5536, #11362, #11299, #12498, #2855, #10522, #704, #891, #7555, #9585, #5594, #1770, #10586, #825, #2605, #1897, #6533, #4761, #6475, #10401, #12377, #8384, #12439, #4695, #12252, #11425, #10337, #1712, #3803, #6718, #1655, #7682, #5718, #763, #9401, #11546, #6654, #6591, #5779, #4572, #3677, #8504, #2733, #9652, #8628, #4634, #10460, #5654, #3555, #3737, #9527, #8444, #960, #7429, #12314, #3613, #7491, #2670, #8568, #7618, #11481, #2792, #1835, #1028, #6095, #11867, #8880, #2157, #2227, #7997, #7743, #10774, #1962, #6908, #2024, #6850, #3867, #3931, #2088, #133, #8693, #6029, #11741, #9840, #11797, #3047, #3104, #6974, #5842, #4054, #198, #10713, #11611, #10912, #5964, #9903, #263, #3, #5905, #10649, #7806, #9713, #7934, #4889, #11678, #1153, #7870, #8814, #8750, #3174, #10843, #8950, #9775, #66, #4119, #9967, #1216, #5015, #5082, #7037, #3992, #1085, #4828, #2984, #4950, #2919, #6782, #8122, #11992 ) ),
 .UNSPECIFIED., .F., .F., .F. ) 
 B_SPLINE_SURFACE_WITH_KNOTS ( ( 2, 2 ),
 ( 3, 2, 2, 2, 2, 2, 2, 2, 2, 2, 2, 2, 2, 2, 2, 2, 2, 2, 2, 2, 2, 2, 2, 2, 2, 2, 2, 2, 2, 2, 2, 2, 2, 2, 2, 2, 2, 2, 2, 2, 2, 2, 2, 2, 2, 2, 2, 2, 2, 2, 2, 2, 2, 2, 2, 2, 2, 2, 2, 2, 2, 2, 2, 2, 2, 2, 2, 2, 2, 2, 2, 2, 2, 2, 2, 2, 2, 2, 2, 2, 2, 2, 2, 2, 2, 2, 2, 2, 2, 2, 2, 2, 2, 2, 2, 2, 2, 2, 2, 2, 2, 2, 2, 2, 2, 2, 2, 2, 2, 2, 2, 2, 2, 2, 2, 2, 2, 2, 2, 2, 2, 2, 2, 2, 2, 2, 2, 2, 2, 2, 2, 2, 2, 2, 2, 2, 2, 2, 2, 2, 2, 2, 2, 2, 2, 2, 2, 2, 2, 2, 3 ),
 ( 0.000000000000000000, 1.000000000000000000 ),
 ( 0.000000000000000000, 0.006666666666666667095, 0.01333333333333333419, 0.02000000000000000042, 0.02666666666666666838, 0.03333333333333333287, 0.04000000000000000083, 0.04666666666666666879, 0.05333333333333333676, 0.05999999999999999778, 0.06666666666666666574, 0.07333333333333333370, 0.08000000000000000167, 0.08666666666666666963, 0.09333333333333333759, 0.1000000000000000056, 0.1066666666666666735, 0.1133333333333333276, 0.1199999999999999956, 0.1266666666666666774, 0.1333333333333333315, 0.1400000000000000133, 0.1466666666666666674, 0.1533333333333333215, 0.1600000000000000033, 0.1666666666666666574, 0.1733333333333333393, 0.1799999999999999933, 0.1866666666666666752, 0.1933333333333333293, 0.2000000000000000111, 0.2066666666666666652, 0.2133333333333333470, 0.2200000000000000011, 0.2266666666666666552, 0.2333333333333333370, 0.2399999999999999911, 0.2466666666666666730, 0.2533333333333333548, 0.2600000000000000089, 0.2666666666666666630, 0.2733333333333333171, 0.2800000000000000266, 0.2866666666666666807, 0.2933333333333333348, 0.2999999999999999889, 0.3066666666666666430, 0.3133333333333333526, 0.3200000000000000067, 0.3266666666666666607, 0.3333333333333333148, 0.3400000000000000244, 0.3466666666666666785, 0.3533333333333333326, 0.3599999999999999867, 0.3666666666666666408, 0.3733333333333333504, 0.3800000000000000044, 0.3866666666666666585, 0.3933333333333333126, 0.4000000000000000222, 0.4066666666666666763, 0.4133333333333333304, 0.4199999999999999845, 0.4266666666666666941, 0.4333333333333333481, 0.4400000000000000022, 0.4466666666666666563, 0.4533333333333333104, 0.4600000000000000200, 0.4666666666666666741, 0.4733333333333333282, 0.4799999999999999822, 0.4866666666666666918, 0.4933333333333333459, 0.5000000000000000000, 0.5066666666666667096, 0.5133333333333333082, 0.5200000000000000178, 0.5266666666666666163, 0.5333333333333333259, 0.5400000000000000355, 0.5466666666666666341, 0.5533333333333333437, 0.5600000000000000533, 0.5666666666666666519, 0.5733333333333333615, 0.5799999999999999600, 0.5866666666666666696, 0.5933333333333333792, 0.5999999999999999778, 0.6066666666666666874, 0.6133333333333332860, 0.6199999999999999956, 0.6266666666666667052, 0.6333333333333333037, 0.6400000000000000133, 0.6466666666666666119, 0.6533333333333333215, 0.6600000000000000311, 0.6666666666666666297, 0.6733333333333333393, 0.6800000000000000488, 0.6866666666666666474, 0.6933333333333333570, 0.6999999999999999556, 0.7066666666666666652, 0.7133333333333333748, 0.7199999999999999734, 0.7266666666666666829, 0.7333333333333332815, 0.7399999999999999911, 0.7466666666666667007, 0.7533333333333332993, 0.7600000000000000089, 0.7666666666666667185, 0.7733333333333333171, 0.7800000000000000266, 0.7866666666666666252, 0.7933333333333333348, 0.8000000000000000444, 0.8066666666666666430, 0.8133333333333333526, 0.8199999999999999512, 0.8266666666666666607, 0.8333333333333333703, 0.8399999999999999689, 0.8466666666666666785, 0.8533333333333333881, 0.8599999999999999867, 0.8666666666666666963, 0.8733333333333332948, 0.8800000000000000044, 0.8866666666666667140, 0.8933333333333333126, 0.9000000000000000222, 0.9066666666666666208, 0.9133333333333333304, 0.9200000000000000400, 0.9266666666666666385, 0.9333333333333333481, 0.9399999999999999467, 0.9466666666666666563, 0.9533333333333333659, 0.9599999999999999645, 0.9666666666666666741, 0.9733333333333333837, 0.9799999999999999822, 0.9866666666666666918, 0.9933333333333332904, 1.000000000000000000 ),
 .UNSPECIFIED. ) 
 GEOMETRIC_REPRESENTATION_ITEM ( )  RATIONAL_B_SPLINE_SURFACE ( (
 ( 1.000000000000000000, 0.9510565162951535312, 1.000000000000000000, 0.9510565162951535312, 1.000000000000000000, 0.9510565162951535312, 1.000000000000000000, 0.9510565162951535312, 1.000000000000000000, 0.9510565162951535312, 1.000000000000000000, 0.9510565162951535312, 1.000000000000000000, 0.9510565162951535312, 1.000000000000000000, 0.9510565162951535312, 1.000000000000000000, 0.9510565162951535312, 1.000000000000000000, 0.9510565162951535312, 1.000000000000000000, 0.9510565162951535312, 1.000000000000000000, 0.9510565162951535312, 1.000000000000000000, 0.9510565162951535312, 1.000000000000000000, 0.9510565162951535312, 1.000000000000000000, 0.9510565162951535312, 1.000000000000000000, 0.9510565162951535312, 1.000000000000000000, 0.9510565162951535312, 1.000000000000000000, 0.9510565162951535312, 1.000000000000000000, 0.9510565162951535312, 1.000000000000000000, 0.9510565162951535312, 1.000000000000000000, 0.9510565162951535312, 1.000000000000000000, 0.9510565162951535312, 1.000000000000000000, 0.9510565162951535312, 1.000000000000000000, 0.9510565162951535312, 1.000000000000000000, 0.9510565162951535312, 1.000000000000000000, 0.9510565162951535312, 1.000000000000000000, 0.9510565162951535312, 1.000000000000000000, 0.9510565162951535312, 1.000000000000000000, 0.9510565162951535312, 1.000000000000000000, 0.9510565162951535312, 1.000000000000000000, 0.9510565162951535312, 1.000000000000000000, 0.9510565162951535312, 1.000000000000000000, 0.9510565162951535312, 1.000000000000000000, 0.9510565162951535312, 1.000000000000000000, 0.9510565162951535312, 1.000000000000000000, 0.9510565162951535312, 1.000000000000000000, 0.9510565162951535312, 1.000000000000000000, 0.9510565162951535312, 1.000000000000000000, 0.9510565162951535312, 1.000000000000000000, 0.9510565162951535312, 1.000000000000000000, 0.9510565162951535312, 1.000000000000000000, 0.9510565162951535312, 1.000000000000000000, 0.9510565162951535312, 1.000000000000000000, 0.9510565162951535312, 1.000000000000000000, 0.9510565162951535312, 1.000000000000000000, 0.9510565162951535312, 1.000000000000000000, 0.9510565162951535312, 1.000000000000000000, 0.9510565162951535312, 1.000000000000000000, 0.9510565162951535312, 1.000000000000000000, 0.9510565162951535312, 1.000000000000000000, 0.9510565162951535312, 1.000000000000000000, 0.9510565162951535312, 1.000000000000000000, 0.9510565162951535312, 1.000000000000000000, 0.9510565162951535312, 1.000000000000000000, 0.9510565162951535312, 1.000000000000000000, 0.9510565162951535312, 1.000000000000000000, 0.9510565162951535312, 1.000000000000000000, 0.9510565162951535312, 1.000000000000000000, 0.9510565162951535312, 1.000000000000000000, 0.9510565162951535312, 1.000000000000000000, 0.9510565162951535312, 1.000000000000000000, 0.9510565162951535312, 1.000000000000000000, 0.9510565162951535312, 1.000000000000000000, 0.9510565162951535312, 1.000000000000000000, 0.9510565162951535312, 1.000000000000000000, 0.9510565162951535312, 1.000000000000000000, 0.9510565162951535312, 1.000000000000000000, 0.9510565162951535312, 1.000000000000000000, 0.9510565162951535312, 1.000000000000000000, 0.9510565162951535312, 1.000000000000000000, 0.9510565162951535312, 1.000000000000000000, 0.9510565162951535312, 1.000000000000000000, 0.9510565162951535312, 1.000000000000000000, 0.9510565162951535312, 1.000000000000000000, 0.9510565162951535312, 1.000000000000000000, 0.9510565162951535312, 1.000000000000000000, 0.9510565162951535312, 1.000000000000000000, 0.9510565162951535312, 1.000000000000000000, 0.9510565162951535312, 1.000000000000000000, 0.9510565162951535312, 1.000000000000000000, 0.9510565162951535312, 1.000000000000000000, 0.9510565162951535312, 1.000000000000000000, 0.9510565162951535312, 1.000000000000000000, 0.9510565162951535312, 1.000000000000000000, 0.9510565162951535312, 1.000000000000000000, 0.9510565162951535312, 1.000000000000000000, 0.9510565162951535312, 1.000000000000000000, 0.9510565162951535312, 1.000000000000000000, 0.9510565162951535312, 1.000000000000000000, 0.9510565162951535312, 1.000000000000000000, 0.9510565162951535312, 1.000000000000000000, 0.9510565162951535312, 1.000000000000000000, 0.9510565162951535312, 1.000000000000000000, 0.9510565162951535312, 1.000000000000000000, 0.9510565162951535312, 1.000000000000000000, 0.9510565162951535312, 1.000000000000000000, 0.9510565162951535312, 1.000000000000000000, 0.9510565162951535312, 1.000000000000000000, 0.9510565162951535312, 1.000000000000000000, 0.9510565162951535312, 1.000000000000000000, 0.9510565162951535312, 1.000000000000000000, 0.9510565162951535312, 1.000000000000000000, 0.9510565162951535312, 1.000000000000000000, 0.9510565162951535312, 1.000000000000000000, 0.9510565162951535312, 1.000000000000000000, 0.9510565162951535312, 1.000000000000000000, 0.9510565162951535312, 1.000000000000000000, 0.9510565162951535312, 1.000000000000000000, 0.9510565162951535312, 1.000000000000000000, 0.9510565162951535312, 1.000000000000000000, 0.9510565162951535312, 1.000000000000000000, 0.9510565162951535312, 1.000000000000000000, 0.9510565162951535312, 1.000000000000000000, 0.9510565162951535312, 1.000000000000000000, 0.9510565162951535312, 1.000000000000000000, 0.9510565162951535312, 1.000000000000000000, 0.9510565162951535312, 1.000000000000000000, 0.9510565162951535312, 1.000000000000000000, 0.9510565162951535312, 1.000000000000000000, 0.9510565162951535312, 1.000000000000000000, 0.9510565162951535312, 1.000000000000000000, 0.9510565162951535312, 1.000000000000000000, 0.9510565162951535312, 1.000000000000000000, 0.9510565162951535312, 1.000000000000000000, 0.9510565162951535312, 1.000000000000000000, 0.9510565162951535312, 1.000000000000000000, 0.9510565162951535312, 1.000000000000000000, 0.9510565162951535312, 1.000000000000000000, 0.9510565162951535312, 1.000000000000000000, 0.9510565162951535312, 1.000000000000000000, 0.9510565162951535312, 1.000000000000000000, 0.9510565162951535312, 1.000000000000000000, 0.9510565162951535312, 1.000000000000000000, 0.9510565162951535312, 1.000000000000000000, 0.9510565162951535312, 1.000000000000000000, 0.9510565162951535312, 1.000000000000000000, 0.9510565162951535312, 1.000000000000000000, 0.9510565162951535312, 1.000000000000000000, 0.9510565162951535312, 1.000000000000000000, 0.9510565162951535312, 1.000000000000000000, 0.9510565162951535312, 1.000000000000000000, 0.9510565162951535312, 1.000000000000000000, 0.9510565162951535312, 1.000000000000000000, 0.9510565162951535312, 1.000000000000000000, 0.9510565162951535312, 1.000000000000000000, 0.9510565162951535312, 1.000000000000000000, 0.9510565162951535312, 1.000000000000000000, 0.9510565162951535312, 1.000000000000000000, 0.9510565162951535312, 1.000000000000000000, 0.9510565162951535312, 1.000000000000000000),
 ( 1.000000000000000000, 0.9510565162951535312, 1.000000000000000000, 0.9510565162951535312, 1.000000000000000000, 0.9510565162951535312, 1.000000000000000000, 0.9510565162951535312, 1.000000000000000000, 0.9510565162951535312, 1.000000000000000000, 0.9510565162951535312, 1.000000000000000000, 0.9510565162951535312, 1.000000000000000000, 0.9510565162951535312, 1.000000000000000000, 0.9510565162951535312, 1.000000000000000000, 0.9510565162951535312, 1.000000000000000000, 0.9510565162951535312, 1.000000000000000000, 0.9510565162951535312, 1.000000000000000000, 0.9510565162951535312, 1.000000000000000000, 0.9510565162951535312, 1.000000000000000000, 0.9510565162951535312, 1.000000000000000000, 0.9510565162951535312, 1.000000000000000000, 0.9510565162951535312, 1.000000000000000000, 0.9510565162951535312, 1.000000000000000000, 0.9510565162951535312, 1.000000000000000000, 0.9510565162951535312, 1.000000000000000000, 0.9510565162951535312, 1.000000000000000000, 0.9510565162951535312, 1.000000000000000000, 0.9510565162951535312, 1.000000000000000000, 0.9510565162951535312, 1.000000000000000000, 0.9510565162951535312, 1.000000000000000000, 0.9510565162951535312, 1.000000000000000000, 0.9510565162951535312, 1.000000000000000000, 0.9510565162951535312, 1.000000000000000000, 0.9510565162951535312, 1.000000000000000000, 0.9510565162951535312, 1.000000000000000000, 0.9510565162951535312, 1.000000000000000000, 0.9510565162951535312, 1.000000000000000000, 0.9510565162951535312, 1.000000000000000000, 0.9510565162951535312, 1.000000000000000000, 0.9510565162951535312, 1.000000000000000000, 0.9510565162951535312, 1.000000000000000000, 0.9510565162951535312, 1.000000000000000000, 0.9510565162951535312, 1.000000000000000000, 0.9510565162951535312, 1.000000000000000000, 0.9510565162951535312, 1.000000000000000000, 0.9510565162951535312, 1.000000000000000000, 0.9510565162951535312, 1.000000000000000000, 0.9510565162951535312, 1.000000000000000000, 0.9510565162951535312, 1.000000000000000000, 0.9510565162951535312, 1.000000000000000000, 0.9510565162951535312, 1.000000000000000000, 0.9510565162951535312, 1.000000000000000000, 0.9510565162951535312, 1.000000000000000000, 0.9510565162951535312, 1.000000000000000000, 0.9510565162951535312, 1.000000000000000000, 0.9510565162951535312, 1.000000000000000000, 0.9510565162951535312, 1.000000000000000000, 0.9510565162951535312, 1.000000000000000000, 0.9510565162951535312, 1.000000000000000000, 0.9510565162951535312, 1.000000000000000000, 0.9510565162951535312, 1.000000000000000000, 0.9510565162951535312, 1.000000000000000000, 0.9510565162951535312, 1.000000000000000000, 0.9510565162951535312, 1.000000000000000000, 0.9510565162951535312, 1.000000000000000000, 0.9510565162951535312, 1.000000000000000000, 0.9510565162951535312, 1.000000000000000000, 0.9510565162951535312, 1.000000000000000000, 0.9510565162951535312, 1.000000000000000000, 0.9510565162951535312, 1.000000000000000000, 0.9510565162951535312, 1.000000000000000000, 0.9510565162951535312, 1.000000000000000000, 0.9510565162951535312, 1.000000000000000000, 0.9510565162951535312, 1.000000000000000000, 0.9510565162951535312, 1.000000000000000000, 0.9510565162951535312, 1.000000000000000000, 0.9510565162951535312, 1.000000000000000000, 0.9510565162951535312, 1.000000000000000000, 0.9510565162951535312, 1.000000000000000000, 0.9510565162951535312, 1.000000000000000000, 0.9510565162951535312, 1.000000000000000000, 0.9510565162951535312, 1.000000000000000000, 0.9510565162951535312, 1.000000000000000000, 0.9510565162951535312, 1.000000000000000000, 0.9510565162951535312, 1.000000000000000000, 0.9510565162951535312, 1.000000000000000000, 0.9510565162951535312, 1.000000000000000000, 0.9510565162951535312, 1.000000000000000000, 0.9510565162951535312, 1.000000000000000000, 0.9510565162951535312, 1.000000000000000000, 0.9510565162951535312, 1.000000000000000000, 0.9510565162951535312, 1.000000000000000000, 0.9510565162951535312, 1.000000000000000000, 0.9510565162951535312, 1.000000000000000000, 0.9510565162951535312, 1.000000000000000000, 0.9510565162951535312, 1.000000000000000000, 0.9510565162951535312, 1.000000000000000000, 0.9510565162951535312, 1.000000000000000000, 0.9510565162951535312, 1.000000000000000000, 0.9510565162951535312, 1.000000000000000000, 0.9510565162951535312, 1.000000000000000000, 0.9510565162951535312, 1.000000000000000000, 0.9510565162951535312, 1.000000000000000000, 0.9510565162951535312, 1.000000000000000000, 0.9510565162951535312, 1.000000000000000000, 0.9510565162951535312, 1.000000000000000000, 0.9510565162951535312, 1.000000000000000000, 0.9510565162951535312, 1.000000000000000000, 0.9510565162951535312, 1.000000000000000000, 0.9510565162951535312, 1.000000000000000000, 0.9510565162951535312, 1.000000000000000000, 0.9510565162951535312, 1.000000000000000000, 0.9510565162951535312, 1.000000000000000000, 0.9510565162951535312, 1.000000000000000000, 0.9510565162951535312, 1.000000000000000000, 0.9510565162951535312, 1.000000000000000000, 0.9510565162951535312, 1.000000000000000000, 0.9510565162951535312, 1.000000000000000000, 0.9510565162951535312, 1.000000000000000000, 0.9510565162951535312, 1.000000000000000000, 0.9510565162951535312, 1.000000000000000000, 0.9510565162951535312, 1.000000000000000000, 0.9510565162951535312, 1.000000000000000000, 0.9510565162951535312, 1.000000000000000000, 0.9510565162951535312, 1.000000000000000000, 0.9510565162951535312, 1.000000000000000000, 0.9510565162951535312, 1.000000000000000000, 0.9510565162951535312, 1.000000000000000000, 0.9510565162951535312, 1.000000000000000000, 0.9510565162951535312, 1.000000000000000000, 0.9510565162951535312, 1.000000000000000000, 0.9510565162951535312, 1.000000000000000000, 0.9510565162951535312, 1.000000000000000000, 0.9510565162951535312, 1.000000000000000000, 0.9510565162951535312, 1.000000000000000000, 0.9510565162951535312, 1.000000000000000000, 0.9510565162951535312, 1.000000000000000000, 0.9510565162951535312, 1.000000000000000000, 0.9510565162951535312, 1.000000000000000000, 0.9510565162951535312, 1.000000000000000000, 0.9510565162951535312, 1.000000000000000000, 0.9510565162951535312, 1.000000000000000000, 0.9510565162951535312, 1.000000000000000000, 0.9510565162951535312, 1.000000000000000000, 0.9510565162951535312, 1.000000000000000000, 0.9510565162951535312, 1.000000000000000000, 0.9510565162951535312, 1.000000000000000000, 0.9510565162951535312, 1.000000000000000000, 0.9510565162951535312, 1.000000000000000000, 0.9510565162951535312, 1.000000000000000000, 0.9510565162951535312, 1.000000000000000000, 0.9510565162951535312, 1.000000000000000000, 0.9510565162951535312, 1.000000000000000000, 0.9510565162951535312, 1.000000000000000000, 0.9510565162951535312, 1.000000000000000000) ) ) 
 REPRESENTATION_ITEM ( '' )  SURFACE ( )  );
#11109 = VECTOR ( 'NONE', #7841, 1000.000000000000000 ) ;
#11110 = CARTESIAN_POINT ( 'NONE',  ( 32.67500000054622689, 15.71886984736413773, 84.90069139318163138 ) ) ;
#11111 = CARTESIAN_POINT ( 'NONE',  ( 5.000000000000000000, 2.342598717236900718, -4.057500000000001883 ) ) ;
#11112 = CARTESIAN_POINT ( 'NONE',  ( 47.47500000054623115, 26.19570976099943849, 95.29460816699764791 ) ) ;
#11113 = CARTESIAN_POINT ( 'NONE',  ( 36.67500000054622689, 15.71886984736413773, 84.90069139318163138 ) ) ;
#11114 = CARTESIAN_POINT ( 'NONE',  ( 33.99999999999998579, 20.00000000000000355, 98.29316153445363113 ) ) ;
#11115 = CARTESIAN_POINT ( 'NONE',  ( 46.97500000054623115, 24.28113015263587471, 84.90069139318163138 ) ) ;
#11116 = ORIENTED_EDGE ( 'NONE', *, *, #7153, .T. ) ;
#11117 = CARTESIAN_POINT ( 'NONE',  ( 22.85000000109246443, 24.40838939219355197, 84.72553407664153724 ) ) ;
#11118 = CARTESIAN_POINT ( 'NONE',  ( -6.106142575418606278, 12.07400325324896784, 24.24423224237354901 ) ) ;
#11119 = VERTEX_POINT ( 'NONE', #12346 ) ;
#11120 = VECTOR ( 'NONE', #9188, 1000.000000000000227 ) ;
#11121 = DIRECTION ( 'NONE',  ( 1.000000000000000000, 0.000000000000000000, 0.000000000000000000 ) ) ;
#11122 = EDGE_LOOP ( 'NONE', ( #1644, #9174, #4997, #10799 ) ) ;
#11123 = CARTESIAN_POINT ( 'NONE',  ( 0.000000000000000000, 0.000000000000000000, 169.9999999999999716 ) ) ;
#11124 = LINE ( 'NONE', #2430, #2625 ) ;
#11125 = LINE ( 'NONE', #6369, #5435 ) ;
#11126 = FACE_OUTER_BOUND ( 'NONE', #3890, .T. ) ;
#11127 = VECTOR ( 'NONE', #10617, 1000.000000000000000 ) ;
#11128 = CARTESIAN_POINT ( 'NONE',  ( 24.77500000054622831, 20.00000000000000355, 83.50966788445364841 ) ) ;
#11129 = CARTESIAN_POINT ( 'NONE',  ( 26.27500000054622475, 13.07298590277314254, 93.04388485072563242 ) ) ;
#11130 = DIRECTION ( 'NONE',  ( -1.000000000000000000, -0.000000000000000000, -0.000000000000000000 ) ) ;
#11131 = VECTOR ( 'NONE', #534, 1000.000000000000000 ) ;
#11132 = CARTESIAN_POINT ( 'NONE',  ( -2.217326200926027724, 45.51555228448187762, 24.90189708455264395 ) ) ;
#11133 = VERTEX_POINT ( 'NONE', #4540 ) ;
#11134 = CARTESIAN_POINT ( 'NONE',  ( 44.65000000109246514, 20.00000000000000355, 83.29316153445364534 ) ) ;
#11135 = CARTESIAN_POINT ( 'NONE',  ( 6.000000000000000000, -2.919948986426525117, 5.057500000000004547 ) ) ;
#11136 = ORIENTED_EDGE ( 'NONE', *, *, #4541, .T. ) ;
#11137 = CARTESIAN_POINT ( 'NONE',  ( 29.65000000109246514, 20.00000000000000355, 98.29316153445363113 ) ) ;
#11138 = ORIENTED_EDGE ( 'NONE', *, *, #10024, .F. ) ;
#11139 = CARTESIAN_POINT ( 'NONE',  ( -5.017800233121429088, 11.34386344135788605, -24.49301625034288321 ) ) ;
#11140 = CARTESIAN_POINT ( 'NONE',  ( 5.029111531688879921, 11.35041964440615914, -24.49069713376460555 ) ) ;
#11141 = PLANE ( 'NONE',  #5216 ) ;
#11142 = CARTESIAN_POINT ( 'NONE',  ( -6.609692946276023662, 12.48878433695339218, 24.11181729628509984 ) ) ;
#11143 = LINE ( 'NONE', #12101, #8485 ) ;
#11144 = VECTOR ( 'NONE', #3682, 1000.000000000000000 ) ;
#11145 = CARTESIAN_POINT ( 'NONE',  ( -6.629750755640679394, 12.48603128090877057, 19.93185325444923706 ) ) ;
#11146 = CARTESIAN_POINT ( 'NONE',  ( -9.106176344275144885, 15.85459820044763823, 26.47820341525681442 ) ) ;
#11147 = ADVANCED_FACE ( 'NONE', ( #927 ), #8660, .F. ) ;
#11148 = DIRECTION ( 'NONE',  ( -0.000000000000000000, -0.000000000000000000, 1.000000000000000000 ) ) ;
#11149 = CARTESIAN_POINT ( 'NONE',  ( -3.973554925899839052, 53.05255087154787219, 24.68288788663009825 ) ) ;
#11150 = ORIENTED_EDGE ( 'NONE', *, *, #12173, .T. ) ;
#11151 =( BOUNDED_CURVE ( )  B_SPLINE_CURVE ( 3, ( #116, #11594, #2068, #2903 ),
 .UNSPECIFIED., .F., .F. ) 
 B_SPLINE_CURVE_WITH_KNOTS ( ( 4, 4 ),
 ( 3.411525449423196132, 4.712388980384689674 ),
 .UNSPECIFIED. ) 
 CURVE ( )  GEOMETRIC_REPRESENTATION_ITEM ( )  RATIONAL_B_SPLINE_CURVE ( ( 1.000000000000000000, 0.8638816171694809753, 0.8638816171694809753, 1.000000000000000000 ) ) 
 REPRESENTATION_ITEM ( '' )  );
#11152 = CIRCLE ( 'NONE', #8126, 5.057500000000000107 ) ;
#11153 = CARTESIAN_POINT ( 'NONE',  ( -2.000000000000015543, 20.00000000000000355, 90.79316153445363113 ) ) ;
#11154 = DIRECTION ( 'NONE',  ( 0.4999999999999892308, 0.000000000000000000, -0.8660254037844448138 ) ) ;
#11155 = CARTESIAN_POINT ( 'NONE',  ( 41.37500000054622973, 27.65831843345427998, 90.79316153445363113 ) ) ;
#11156 = CARTESIAN_POINT ( 'NONE',  ( 28.07500000054622902, 13.80429023900056507, 95.29460816699764791 ) ) ;
#11157 = CARTESIAN_POINT ( 'NONE',  ( 0.000000000000000000, 2.919948986426540660, 5.057499999999996554 ) ) ;
#11158 = CARTESIAN_POINT ( 'NONE',  ( -6.999999999999999112, 92.00000000000000000, 69.99999999999998579 ) ) ;
#11159 = LINE ( 'NONE', #10153, #5364 ) ;
#11160 = DIRECTION ( 'NONE',  ( 0.000000000000000000, 0.000000000000000000, -1.000000000000000000 ) ) ;
#11161 = ORIENTED_EDGE ( 'NONE', *, *, #12116, .T. ) ;
#11162 = CIRCLE ( 'NONE', #11373, 21.00000000000000000 ) ;
#11163 = CARTESIAN_POINT ( 'NONE',  ( -3.594513446512490388E-16, 55.00000000000000000, -21.00000000000000000 ) ) ;
#11164 = ORIENTED_EDGE ( 'NONE', *, *, #10691, .F. ) ;
#11165 = CARTESIAN_POINT ( 'NONE',  ( 48.65000000109246514, 20.00000000000000355, 83.29316153445364534 ) ) ;
#11166 = EDGE_CURVE ( 'NONE', #1979, #12014, #4969, .T. ) ;
#11167 = ORIENTED_EDGE ( 'NONE', *, *, #7518, .F. ) ;
#11168 = ADVANCED_FACE ( 'NONE', ( #5506 ), #9373, .F. ) ;
#11169 =( BOUNDED_CURVE ( )  B_SPLINE_CURVE ( 2, ( #159, #7958, #4082, #7186, #1301, #1179, #410, #11000, #10801, #2310, #9040 ),
 .UNSPECIFIED., .F., .F. ) 
 B_SPLINE_CURVE_WITH_KNOTS ( ( 3, 2, 2, 2, 2, 3 ),
 ( 0.8000000000000000444, 0.8066666666666666430, 0.8133333333333333526, 0.8199999999999999512, 0.8266666666666666607, 0.8333333333333333703 ),
 .UNSPECIFIED. ) 
 CURVE ( )  GEOMETRIC_REPRESENTATION_ITEM ( )  RATIONAL_B_SPLINE_CURVE ( ( 1.000000000000000000, 0.9510565162951535312, 1.000000000000000000, 0.9510565162951535312, 1.000000000000000000, 0.9510565162951535312, 1.000000000000000000, 0.9510565162951535312, 1.000000000000000000, 0.9510565162951535312, 1.000000000000000000 ) ) 
 REPRESENTATION_ITEM ( '' )  );
#11170 =( NAMED_UNIT ( * ) PLANE_ANGLE_UNIT ( ) SI_UNIT ( $, .RADIAN. ) );
#11171 = CARTESIAN_POINT ( 'NONE',  ( 32.47500000054621694, 13.07298590277314432, 88.54243821818161564 ) ) ;
#11172 = DIRECTION ( 'NONE',  ( 0.000000000000000000, 0.8660254037844379305, -0.5000000000000012212 ) ) ;
#11173 = EDGE_CURVE ( 'NONE', #2795, #10888, #8912, .T. ) ;
#11174 = CARTESIAN_POINT ( 'NONE',  ( 44.87500000054623683, 22.36655054427230382, 83.50966788445364841 ) ) ;
#11175 = CARTESIAN_POINT ( 'NONE',  ( 36.57500000054621125, 13.80429023900056684, 86.29171490190961435 ) ) ;
#11176 = CARTESIAN_POINT ( 'NONE',  ( 36.89999999999997726, 17.56310227825321135, 83.29316153445363113 ) ) ;
#11177 = CARTESIAN_POINT ( 'NONE',  ( -5.029901707005755895, 28.64912781045596901, 20.39087425871785086 ) ) ;
#11178 = CARTESIAN_POINT ( 'NONE',  ( 46.17500000054623399, 13.07298590277314254, 93.04388485072563242 ) ) ;
#11179 = ORIENTED_EDGE ( 'NONE', *, *, #6658, .T. ) ;
#11180 = CARTESIAN_POINT ( 'NONE',  ( 27.25000000109246656, 27.13292387221364876, 93.11078899226573924 ) ) ;
#11181 = CARTESIAN_POINT ( 'NONE',  ( -9.106574839427329593, 15.85560948713796492, 23.28279145951148266 ) ) ;
#11182 = ORIENTED_EDGE ( 'NONE', *, *, #12244, .F. ) ;
#11183 = EDGE_CURVE ( 'NONE', #6466, #4258, #4088, .T. ) ;
#11184 = FACE_OUTER_BOUND ( 'NONE', #8333, .T. ) ;
#11185 = ORIENTED_EDGE ( 'NONE', *, *, #12344, .T. ) ;
#11186 = DIRECTION ( 'NONE',  ( 0.000000000000000000, 0.000000000000000000, -1.000000000000000000 ) ) ;
#11187 = CYLINDRICAL_SURFACE ( 'NONE', #8105, 26.49999999999999645 ) ;
#11188 = CYLINDRICAL_SURFACE ( 'NONE', #11702, 26.49999999999999645 ) ;
#11189 = EDGE_CURVE ( 'NONE', #2911, #8038, #6192, .T. ) ;
#11190 = CARTESIAN_POINT ( 'NONE',  ( 27.37500000054622973, 26.92701409722686634, 93.04388485072563242 ) ) ;
#11191 = CARTESIAN_POINT ( 'NONE',  ( 26.77500000054622475, 17.63344945572770328, 83.50966788445364841 ) ) ;
#11192 = LINE ( 'NONE', #8156, #11026 ) ;
#11193 = LINE ( 'NONE', #8097, #3210 ) ;
#11194 = VERTEX_POINT ( 'NONE', #1929 ) ;
#11195 = FILL_AREA_STYLE_COLOUR ( '', #11721 ) ;
#11196 = VERTEX_POINT ( 'NONE', #5999 ) ;
#11197 = CARTESIAN_POINT ( 'NONE',  ( 30.25000000109246656, 12.86707612778636012, 88.47553407664152303 ) ) ;
#11198 = ORIENTED_EDGE ( 'NONE', *, *, #3891, .F. ) ;
#11199 = CARTESIAN_POINT ( 'NONE',  ( -6.608660176926854923, 12.46713484822145190, -24.11541629257941111 ) ) ;
#11200 = CARTESIAN_POINT ( 'NONE',  ( 8.919948986426568638, 0.000000000000000000, 0.000000000000000000 ) ) ;
#11201 = CARTESIAN_POINT ( 'NONE',  ( 20.57500000054622902, 15.71886984736413773, 84.90069139318163138 ) ) ;
#11202 = TOROIDAL_SURFACE ( 'NONE', #3094, 6.600000000000003197, 0.5999999999999999778 ) ;
#11203 = DIRECTION ( 'NONE',  ( 0.000000000000000000, -1.000000000000000000, 0.000000000000000000 ) ) ;
#11204 = FACE_OUTER_BOUND ( 'NONE', #9162, .T. ) ;
#11205 = CARTESIAN_POINT ( 'NONE',  ( -6.840285088253086343, 12.69813275654655094, 27.15267049763187401 ) ) ;
#11206 = CARTESIAN_POINT ( 'NONE',  ( 12.00000000000000000, 0.000000000000000000, -6.600000000000003197 ) ) ;
#11207 = CONICAL_SURFACE ( 'NONE', #7771, 5.035999999999999588, 0.7853981633974685961 ) ;
#11208 = CARTESIAN_POINT ( 'NONE',  ( 47.05000000109247082, 27.13292387221364876, 88.47553407664153724 ) ) ;
#11209 = VERTEX_POINT ( 'NONE', #8979 ) ;
#11210 = EDGE_CURVE ( 'NONE', #6725, #3445, #1882, .T. ) ;
#11211 = CARTESIAN_POINT ( 'NONE',  ( 6.000000000000000000, 2.919948986426538884, 5.057499999999996554 ) ) ;
#11212 = EDGE_CURVE ( 'NONE', #5229, #2895, #9457, .T. ) ;
#11213 = DIRECTION ( 'NONE',  ( 0.000000000000000000, -0.000000000000000000, 1.000000000000000000 ) ) ;
#11214 = CARTESIAN_POINT ( 'NONE',  ( 39.07500000054622546, 24.28113015263587471, 84.90069139318163138 ) ) ;
#11215 = VECTOR ( 'NONE', #6813, 1000.000000000000000 ) ;
#11216 = CARTESIAN_POINT ( 'NONE',  ( 28.47500000054622760, 13.80429023900056684, 86.29171490190961435 ) ) ;
#11217 = CARTESIAN_POINT ( 'NONE',  ( 7.146575930227264450, 13.00402921949032731, 93.50701428624745404 ) ) ;
#11218 = DIRECTION ( 'NONE',  ( -0.000000000000000000, -1.000000000000000000, -0.000000000000000000 ) ) ;
#11219 = AXIS2_PLACEMENT_3D ( 'NONE', #3124, #9858, #2175 ) ;
#11220 = ORIENTED_EDGE ( 'NONE', *, *, #10099, .F. ) ;
#11221 = CARTESIAN_POINT ( 'NONE',  ( 34.99999999999999289, 20.00000000000000355, 83.29316153445364534 ) ) ;
#11222 = ORIENTED_EDGE ( 'NONE', *, *, #12102, .T. ) ;
#11223 = CARTESIAN_POINT ( 'NONE',  ( -50.00000000000001421, 18.00000000000000355, 152.2284161474004520 ) ) ;
#11224 = ORIENTED_EDGE ( 'NONE', *, *, #10950, .T. ) ;
#11225 = DIRECTION ( 'NONE',  ( -0.000000000000000000, -0.000000000000000000, 1.000000000000000000 ) ) ;
#11226 = DIRECTION ( 'NONE',  ( 0.000000000000000000, 0.000000000000000000, 1.000000000000000000 ) ) ;
#11227 = VECTOR ( 'NONE', #182, 1000.000000000000000 ) ;
#11228 = CARTESIAN_POINT ( 'NONE',  ( 30.47500000054622404, 13.07298590277314432, 88.54243821818161564 ) ) ;
#11229 = PLANE ( 'NONE',  #4109 ) ;
#11230 = CARTESIAN_POINT ( 'NONE',  ( 46.37500000054622973, 13.07298590277314432, 88.54243821818161564 ) ) ;
#11231 = CARTESIAN_POINT ( 'NONE',  ( 35.37500000054622973, 27.65831843345427998, 90.79316153445363113 ) ) ;
#11232 = CARTESIAN_POINT ( 'NONE',  ( 36.49999999999998579, 12.11403331821300533, 90.79316153445363113 ) ) ;
#11233 = EDGE_CURVE ( 'NONE', #2882, #6159, #7256, .T. ) ;
#11234 = CARTESIAN_POINT ( 'NONE',  ( 6.611279324052055095, 27.53068265742442122, 24.11471400905219298 ) ) ;
#11235 = CARTESIAN_POINT ( 'NONE',  ( 37.97500000054623115, 15.71886984736413417, 96.68563167572563088 ) ) ;
#11236 = ORIENTED_EDGE ( 'NONE', *, *, #8321, .T. ) ;
#11237 =( GEOMETRIC_REPRESENTATION_CONTEXT ( 3 ) GLOBAL_UNCERTAINTY_ASSIGNED_CONTEXT ( ( #8686 ) ) GLOBAL_UNIT_ASSIGNED_CONTEXT ( ( #4130, #11620, #5026 ) ) REPRESENTATION_CONTEXT ( 'NONE', 'WORKASPACE' ) );
#11238 = CARTESIAN_POINT ( 'NONE',  ( 45.67500000054621978, 22.36655054427230027, 98.07665518445361386 ) ) ;
#11239 = DIRECTION ( 'NONE',  ( 0.000000000000000000, 0.000000000000000000, 1.000000000000000000 ) ) ;
#11240 = ORIENTED_EDGE ( 'NONE', *, *, #3273, .T. ) ;
#11241 = CARTESIAN_POINT ( 'NONE',  ( -6.605663331672668726, 27.51475609591144789, 27.21088142802653920 ) ) ;
#11242 = EDGE_CURVE ( 'NONE', #12320, #2108, #6564, .T. ) ;
#11243 = ORIENTED_EDGE ( 'NONE', *, *, #7190, .F. ) ;
#11244 = PLANE ( 'NONE',  #6173 ) ;
#11245 = CARTESIAN_POINT ( 'NONE',  ( 4.999999999999997335, 20.00000000000000000, 137.5000000000000000 ) ) ;
#11246 = CARTESIAN_POINT ( 'NONE',  ( 36.99999999999999289, 20.00000000000000355, 171.0000000000000000 ) ) ;
#11247 = CIRCLE ( 'NONE', #2130, 8.000000000000000000 ) ;
#11248 = CARTESIAN_POINT ( 'NONE',  ( 32.55000000109247082, 17.56310227825320425, 83.29316153445363113 ) ) ;
#11249 = CARTESIAN_POINT ( 'NONE',  ( 26.47500000054623115, 13.80429023900056684, 86.29171490190961435 ) ) ;
#11250 = CARTESIAN_POINT ( 'NONE',  ( 23.37500000054621907, 27.65831843345427998, 90.79316153445363113 ) ) ;
#11251 = DIRECTION ( 'NONE',  ( 1.000000000000000000, -0.000000000000000000, -0.000000000000000000 ) ) ;
#11252 = CARTESIAN_POINT ( 'NONE',  ( 6.000000000000000000, 2.919948986426526005, -5.057500000000003659 ) ) ;
#11253 = ORIENTED_EDGE ( 'NONE', *, *, #4726, .F. ) ;
#11254 = CIRCLE ( 'NONE', #5990, 5.000000000000000888 ) ;
#11255 = CARTESIAN_POINT ( 'NONE',  ( 36.85000000109246798, 24.40838939219355197, 84.72553407664153724 ) ) ;
#11256 = FACE_OUTER_BOUND ( 'NONE', #5088, .T. ) ;
#11257 = B_SPLINE_CURVE_WITH_KNOTS ( 'NONE', 3,
 ( #6463, #7478, #10323, #11351, #6520, #5437, #2511, #1500, #9120, #3280, #9307, #6257, #6384, #2329, #6195, #11079, #3399, #2386, #12035, #4290, #5314, #9246, #3338, #11264, #10191, #7202, #428, #10135 ),
 .UNSPECIFIED., .F., .F.,
 ( 4, 2, 2, 2, 2, 2, 2, 2, 2, 2, 2, 2, 2, 4 ),
 ( 0.03159723681526421801, 0.03258403062298791120, 0.03357082443071160438, 0.03554441204615898381, 0.03653120585388267699, 0.03751799966160637018, 0.03850479346933006336, 0.03949158727705375654, 0.04146517489250114985, 0.04245196870022484303, 0.04343876250794853622, 0.04541235012339592259, 0.04639914393111962271, 0.04738593773884331589 ),
 .UNSPECIFIED. ) ;
#11258 = ORIENTED_EDGE ( 'NONE', *, *, #60, .T. ) ;
#11259 = CARTESIAN_POINT ( 'NONE',  ( 5.000000000000000000, 3.513898075855364400, 2.028749999999996945 ) ) ;
#11260 = ADVANCED_BREP_SHAPE_REPRESENTATION ( '', ( #10571, #9021 ), #11237 ) ;
#11261 = ADVANCED_FACE ( 'NONE', ( #6246 ), #8094, .F. ) ;
#11262 = VERTEX_POINT ( 'NONE', #9997 ) ;
#11263 = CARTESIAN_POINT ( 'NONE',  ( 33.65000000109246514, 20.00000000000000355, 98.29316153445363113 ) ) ;
#11264 = CARTESIAN_POINT ( 'NONE',  ( -1.651830483015944262, 29.86811216670179903, 24.94746627493933744 ) ) ;
#11265 = CARTESIAN_POINT ( 'NONE',  ( 19.77500000054622831, 20.00000000000000355, 98.07665518445361386 ) ) ;
#11266 = ADVANCED_FACE ( 'NONE', ( #3269 ), #1555, .T. ) ;
#11267 = CIRCLE ( 'NONE', #3168, 10.00000000000000178 ) ;
#11268 = CARTESIAN_POINT ( 'NONE',  ( 38.05000000109246372, 12.86707612778636012, 93.11078899226572503 ) ) ;
#11269 = DIRECTION ( 'NONE',  ( 0.000000000000000000, -1.000000000000000000, -0.000000000000000000 ) ) ;
#11270 = CARTESIAN_POINT ( 'NONE',  ( -8.963542696543054689, 15.55476857908299237, 18.99166849128095791 ) ) ;
#11271 = DIRECTION ( 'NONE',  ( -1.000000000000000000, -0.000000000000000000, -0.000000000000000000 ) ) ;
#11272 = CARTESIAN_POINT ( 'NONE',  ( 26.47500000054623115, 13.80429023900056684, 86.29171490190961435 ) ) ;
#11273 = DIRECTION ( 'NONE',  ( 0.000000000000000000, -1.000000000000000000, 0.000000000000000000 ) ) ;
#11274 = DIRECTION ( 'NONE',  ( 0.000000000000000000, 1.000000000000000000, 0.000000000000000000 ) ) ;
#11275 = VERTEX_POINT ( 'NONE', #1435 ) ;
#11276 = AXIS2_PLACEMENT_3D ( 'NONE', #11780, #9821, #4998 ) ;
#11277 = DIRECTION ( 'NONE',  ( 1.000000000000000000, 0.000000000000000000, -0.000000000000000000 ) ) ;
#11278 = FACE_OUTER_BOUND ( 'NONE', #12134, .T. ) ;
#11279 = CARTESIAN_POINT ( 'NONE',  ( 38.17500000054622689, 13.07298590277314254, 93.04388485072563242 ) ) ;
#11280 = CARTESIAN_POINT ( 'NONE',  ( 37.57500000054623257, 26.19570976099943493, 95.29460816699764791 ) ) ;
#11281 = VECTOR ( 'NONE', #1044, 1000.000000000000000 ) ;
#11282 = CARTESIAN_POINT ( 'NONE',  ( 28.67500000054623044, 17.63344945572770328, 83.50966788445364841 ) ) ;
#11283 = CARTESIAN_POINT ( 'NONE',  ( 5.000000000000000000, -2.342598717236902051, 4.057500000000004547 ) ) ;
#11284 = CARTESIAN_POINT ( 'NONE',  ( 0.000000000000000000, 5.839897972853064445, -8.673617379884035472E-15 ) ) ;
#11285 =( REPRESENTATION_RELATIONSHIP ('NONE','NONE', #4262, #8561 ) REPRESENTATION_RELATIONSHIP_WITH_TRANSFORMATION ( #1334 )SHAPE_REPRESENTATION_RELATIONSHIP( ) );
#11286 = DIRECTION ( 'NONE',  ( 0.000000000000000000, 0.000000000000000000, -1.000000000000000000 ) ) ;
#11287 = CARTESIAN_POINT ( 'NONE',  ( 31.39999999999998437, 27.13292387221364876, 88.47553407664153724 ) ) ;
#11288 = ORIENTED_EDGE ( 'NONE', *, *, #5683, .T. ) ;
#11289 = CARTESIAN_POINT ( 'NONE',  ( -31.74999999999995737, 7.347880794884119736E-16, -6.000000000000000000 ) ) ;
#11290 = ORIENTED_EDGE ( 'NONE', *, *, #2857, .T. ) ;
#11291 = ADVANCED_FACE ( 'NONE', ( #9236 ), #11961, .T. ) ;
#11292 = DIRECTION ( 'NONE',  ( 0.000000000000000000, -1.000000000000000000, 0.000000000000000000 ) ) ;
#11293 = VECTOR ( 'NONE', #11001, 1000.000000000000000 ) ;
#11294 = DIRECTION ( 'NONE',  ( 1.000000000000000000, 0.000000000000000000, 0.000000000000000000 ) ) ;
#11295 = CARTESIAN_POINT ( 'NONE',  ( 30.77500000054622120, 17.63344945572770328, 83.50966788445364841 ) ) ;
#11296 = CARTESIAN_POINT ( 'NONE',  ( 27.05000000109246372, 27.13292387221364876, 88.47553407664153724 ) ) ;
#11297 = CARTESIAN_POINT ( 'NONE',  ( 44.37500000054622973, 13.07298590277314432, 88.54243821818161564 ) ) ;
#11298 = CARTESIAN_POINT ( 'NONE',  ( 34.97500000054622404, 22.36655054427230382, 83.50966788445364841 ) ) ;
#11299 = CARTESIAN_POINT ( 'NONE',  ( 32.59999999999998721, 12.86707612778636012, 88.47553407664152303 ) ) ;
#11300 = B_SPLINE_CURVE_WITH_KNOTS ( 'NONE', 3,
 ( #7608, #1016, #5830, #3857, #5770, #4877, #9639, #8682, #6773, #7734, #10638, #9701, #8742, #4299, #11918, #8999, #10079, #12044, #10762, #9828, #10968, #376, #2073, #5004, #7985, #4176 ),
 .UNSPECIFIED., .F., .F.,
 ( 4, 2, 2, 2, 2, 2, 2, 2, 2, 2, 2, 2, 4 ),
 ( 0.04761567710518913032, 0.04860603727850610484, 0.04959639745182307935, 0.05157711779845704225, 0.05256747797177403064, 0.05355783814509101903, 0.05454819831840800742, 0.05553855849172499581, 0.05751927883835896566, 0.05850963901167595405, 0.05949999918499294244, 0.06148071953162691228, 0.06346143987826088906 ),
 .UNSPECIFIED. ) ;
#11301 = CARTESIAN_POINT ( 'NONE',  ( 0.000000000000000000, 1.065442715258197248E-15, -8.400000000000000355 ) ) ;
#11302 = CARTESIAN_POINT ( 'NONE',  ( 42.17500000054622689, 13.07298590277314254, 93.04388485072563242 ) ) ;
#11303 = ORIENTED_EDGE ( 'NONE', *, *, #2188, .T. ) ;
#11304 = CARTESIAN_POINT ( 'NONE',  ( 20.85000000109246443, 24.40838939219355197, 84.72553407664153724 ) ) ;
#11305 = CARTESIAN_POINT ( 'NONE',  ( 0.6000000000000033085, 0.000000000000000000, 8.400000000000000355 ) ) ;
#11306 = VERTEX_POINT ( 'NONE', #9047 ) ;
#11307 = EDGE_CURVE ( 'NONE', #12230, #6159, #4315, .T. ) ;
#11308 = CARTESIAN_POINT ( 'NONE',  ( -1.320906402760432918, 29.93395141324767295, -27.97622082073361227 ) ) ;
#11309 = ORIENTED_EDGE ( 'NONE', *, *, #3123, .F. ) ;
#11310 = VECTOR ( 'NONE', #2219, 999.9999999999998863 ) ;
#11311 = CARTESIAN_POINT ( 'NONE',  ( 21.20617189303578698, 14.62220435867159374, 151.2938281069642130 ) ) ;
#11312 = EDGE_CURVE ( 'NONE', #12151, #7259, #12087, .T. ) ;
#11313 = CARTESIAN_POINT ( 'NONE',  ( 10.00000000000000355, 20.00000000000000355, 109.9999999999999858 ) ) ;
#11314 = CARTESIAN_POINT ( 'NONE',  ( 20.49999999999998224, 12.11403331821300533, 90.79316153445363113 ) ) ;
#11315 = CARTESIAN_POINT ( 'NONE',  ( 24.37500000054622618, 13.07298590277314432, 88.54243821818161564 ) ) ;
#11316 = CARTESIAN_POINT ( 'NONE',  ( 26.07500000054622546, 15.71886984736413417, 96.68563167572563088 ) ) ;
#11317 = CARTESIAN_POINT ( 'NONE',  ( 12.59999999999999964, 0.000000000000000000, 0.000000000000000000 ) ) ;
#11318 = CARTESIAN_POINT ( 'NONE',  ( 6.000000000000000000, 2.919948986426526005, -5.057500000000003659 ) ) ;
#11319 = VECTOR ( 'NONE', #1915, 1000.000000000000000 ) ;
#11320 = ORIENTED_EDGE ( 'NONE', *, *, #5045, .F. ) ;
#11321 = CARTESIAN_POINT ( 'NONE',  ( 37.15000000109246514, 27.88596668178699645, 90.79316153445363113 ) ) ;
#11322 = CARTESIAN_POINT ( 'NONE',  ( 7.514434402675104430, 13.39403693888593772, 23.84492327520115396 ) ) ;
#11323 = ORIENTED_EDGE ( 'NONE', *, *, #10523, .F. ) ;
#11324 = CARTESIAN_POINT ( 'NONE',  ( 12.00000000000000178, 0.000000000000000000, 0.000000000000000000 ) ) ;
#11325 = ORIENTED_EDGE ( 'NONE', *, *, #11082, .T. ) ;
#11326 = CARTESIAN_POINT ( 'NONE',  ( 1.615667985723896471, 54.74301895128219542, 20.93994550997156168 ) ) ;
#11327 = EDGE_CURVE ( 'NONE', #9848, #5337, #3456, .T. ) ;
#11328 = EDGE_CURVE ( 'NONE', #10732, #5816, #7586, .T. ) ;
#11329 = CARTESIAN_POINT ( 'NONE',  ( 31.15000000109246159, 27.88596668178699645, 90.79316153445363113 ) ) ;
#11330 = AXIS2_PLACEMENT_3D ( 'NONE', #10559, #11269, #9435 ) ;
#11331 = CARTESIAN_POINT ( 'NONE',  ( -50.00000000000001421, 18.00000000000000355, 152.2284161474004520 ) ) ;
#11332 = VECTOR ( 'NONE', #11779, 999.9999999999998863 ) ;
#11333 = VECTOR ( 'NONE', #4534, 1000.000000000000000 ) ;
#11334 = EDGE_CURVE ( 'NONE', #5416, #1035, #11192, .T. ) ;
#11335 = CARTESIAN_POINT ( 'NONE',  ( 3.061616997868383043E-15, 139.9999999999999716, 25.00000000000000000 ) ) ;
#11336 = CARTESIAN_POINT ( 'NONE',  ( 0.000000000000000000, 139.9999999999999716, -25.00000000000000000 ) ) ;
#11337 = DIRECTION ( 'NONE',  ( 0.000000000000000000, 0.000000000000000000, -1.000000000000000000 ) ) ;
#11338 = DIRECTION ( 'NONE',  ( -1.000000000000000000, -0.000000000000000000, -0.000000000000000000 ) ) ;
#11339 = CARTESIAN_POINT ( 'NONE',  ( 47.67500000054622689, 24.28113015263587116, 96.68563167572563088 ) ) ;
#11340 = CARTESIAN_POINT ( 'NONE',  ( 44.99999999999996447, 20.00000000000000355, 162.0000000000000000 ) ) ;
#11341 = PLANE ( 'NONE',  #15 ) ;
#11342 = ORIENTED_EDGE ( 'NONE', *, *, #6815, .T. ) ;
#11343 = ADVANCED_FACE ( 'NONE', ( #7069 ), #2259, .T. ) ;
#11344 = CARTESIAN_POINT ( 'NONE',  ( 0.6522419138580031195, 45.03179559853693092, 24.99358091562669060 ) ) ;
#11345 = CONICAL_SURFACE ( 'NONE', #2634, 26.49999999999999645, 0.7853981633974517207 ) ;
#11346 = CARTESIAN_POINT ( 'NONE',  ( 32.00000000000000000, 6.757601037695096551E-16, -5.035999999999999588 ) ) ;
#11347 = CARTESIAN_POINT ( 'NONE',  ( 34.47500000054623115, 13.80429023900056684, 86.29171490190961435 ) ) ;
#11348 = CARTESIAN_POINT ( 'NONE',  ( 35.27500000054622120, 26.92701409722686634, 88.54243821818162985 ) ) ;
#11349 = CARTESIAN_POINT ( 'NONE',  ( 21.97500000054622760, 15.71886984736413417, 96.68563167572563088 ) ) ;
#11350 = FACE_OUTER_BOUND ( 'NONE', #3147, .T. ) ;
#11351 = CARTESIAN_POINT ( 'NONE',  ( -9.918452521082530282, 21.31677563331469116, 22.94832388515032662 ) ) ;
#11352 = CARTESIAN_POINT ( 'NONE',  ( -2.000000000000015543, 20.00000000000000355, 90.79316153445363113 ) ) ;
#11353 = DIRECTION ( 'NONE',  ( 0.000000000000000000, 0.000000000000000000, 1.000000000000000000 ) ) ;
#11354 = CARTESIAN_POINT ( 'NONE',  ( 9.659257073854845999, 17.39080730681331488, 23.05883108104414347 ) ) ;
#11355 = ORIENTED_EDGE ( 'NONE', *, *, #2114, .T. ) ;
#11356 = VECTOR ( 'NONE', #10764, 1000.000000000000000 ) ;
#11357 = DIRECTION ( 'NONE',  ( 0.000000000000000000, 0.000000000000000000, 1.000000000000000000 ) ) ;
#11358 = CARTESIAN_POINT ( 'NONE',  ( 25.17500000054622689, 26.19570976099943849, 86.29171490190961435 ) ) ;
#11359 = CARTESIAN_POINT ( 'NONE',  ( 6.000000000000000000, -2.919948986426525117, 5.057500000000004547 ) ) ;
#11360 = CARTESIAN_POINT ( 'NONE',  ( 46.27500000054622120, 12.34168156654572357, 90.79316153445363113 ) ) ;
#11361 = CARTESIAN_POINT ( 'NONE',  ( 27.27500000054622475, 26.92701409722686634, 88.54243821818162985 ) ) ;
#11362 = CARTESIAN_POINT ( 'NONE',  ( 32.69999999999999574, 13.62011893735971135, 86.15790661882942914 ) ) ;
#11363 = CIRCLE ( 'NONE', #5897, 25.49999999999998934 ) ;
#11364 = CARTESIAN_POINT ( 'NONE',  ( 9.983143436873248788, 20.66859359106200955, 22.92025639428880623 ) ) ;
#11365 = CARTESIAN_POINT ( 'NONE',  ( 40.07500000054623257, 13.80429023900056507, 95.29460816699764791 ) ) ;
#11366 = VERTEX_POINT ( 'NONE', #2810 ) ;
#11367 = CARTESIAN_POINT ( 'NONE',  ( 47.47500000054623115, 26.19570976099943493, 95.29460816699764791 ) ) ;
#11368 = CARTESIAN_POINT ( 'NONE',  ( -27.49999999999999645, 20.00000000000000355, 169.9999999999999716 ) ) ;
#11369 = ORIENTED_EDGE ( 'NONE', *, *, #2008, .T. ) ;
#11370 = DIRECTION ( 'NONE',  ( -1.000000000000000000, -0.000000000000000000, -0.000000000000000000 ) ) ;
#11371 = ORIENTED_EDGE ( 'NONE', *, *, #11999, .F. ) ;
#11372 = CARTESIAN_POINT ( 'NONE',  ( 6.099398173400666145, 27.93114403207803420, -24.24592268179950594 ) ) ;
#11373 = AXIS2_PLACEMENT_3D ( 'NONE', #5848, #10781, #72 ) ;
#11374 = CARTESIAN_POINT ( 'NONE',  ( 27.50000000000000355, 12.50000000000001066, 145.0000000000000000 ) ) ;
#11375 = CARTESIAN_POINT ( 'NONE',  ( -7.000000000000006217, 84.49999999999998579, 146.8533255156881978 ) ) ;
#11376 = CARTESIAN_POINT ( 'NONE',  ( 43.77500000054621410, 22.36655054427230027, 98.07665518445361386 ) ) ;
#11377 = FACE_OUTER_BOUND ( 'NONE', #6423, .T. ) ;
#11378 = EDGE_CURVE ( 'NONE', #3577, #9159, #1700, .T. ) ;
#11379 = CARTESIAN_POINT ( 'NONE',  ( 23.67500000054622333, 22.36655054427230027, 98.07665518445361386 ) ) ;
#11380 = CARTESIAN_POINT ( 'NONE',  ( 48.39999999999999147, 12.86707612778636012, 93.11078899226572503 ) ) ;
#11381 = CARTESIAN_POINT ( 'NONE',  ( -3.304393266822325703, 46.23318141187127139, 24.78176792680001839 ) ) ;
#11382 = ORIENTED_EDGE ( 'NONE', *, *, #796, .F. ) ;
#11383 = CARTESIAN_POINT ( 'NONE',  ( 38.45000000109246230, 15.59161060780646046, 84.72553407664153724 ) ) ;
#11384 = ORIENTED_EDGE ( 'NONE', *, *, #2837, .T. ) ;
#11385 = ADVANCED_FACE ( 'NONE', ( #661 ), #9603, .F. ) ;
#11386 = EDGE_LOOP ( 'NONE', ( #3901, #6792, #10036, #3458 ) ) ;
#11387 = CARTESIAN_POINT ( 'NONE',  ( 4.838482977639748661, 51.30270979396780717, 20.43510396060395706 ) ) ;
#11388 = CARTESIAN_POINT ( 'NONE',  ( -1.297374591076399408, 54.83977433137422253, -24.96837001061641104 ) ) ;
#11389 = CARTESIAN_POINT ( 'NONE',  ( -7.519134213638725583, 26.60056234660722652, 23.84343405217310874 ) ) ;
#11390 = DIRECTION ( 'NONE',  ( -0.000000000000000000, -0.000000000000000000, 1.000000000000000000 ) ) ;
#11391 = LINE ( 'NONE', #10308, #7476 ) ;
#11392 = ORIENTED_EDGE ( 'NONE', *, *, #139, .T. ) ;
#11393 = EDGE_CURVE ( 'NONE', #5036, #9553, #6167, .T. ) ;
#11394 = CARTESIAN_POINT ( 'NONE',  ( 3.061617454482527662E-15, 30.00000000000001066, 25.00000000000000000 ) ) ;
#11395 = CARTESIAN_POINT ( 'NONE',  ( -0.6613819929564737077, 10.01636118122183028, 27.99414392723079459 ) ) ;
#11396 = CARTESIAN_POINT ( 'NONE',  ( 49.87500000054622262, 20.00000000000000355, 98.07665518445361386 ) ) ;
#11397 = DIRECTION ( 'NONE',  ( -1.000000000000000000, 0.000000000000000000, -0.000000000000000000 ) ) ;
#11398 = CARTESIAN_POINT ( 'NONE',  ( 46.85000000109246798, 24.40838939219355197, 84.72553407664153724 ) ) ;
#11399 = ORIENTED_EDGE ( 'NONE', *, *, #10476, .F. ) ;
#11400 = ORIENTED_EDGE ( 'NONE', *, *, #11242, .T. ) ;
#11401 = AXIS2_PLACEMENT_3D ( 'NONE', #9665, #5094, #6988 ) ;
#11402 = CARTESIAN_POINT ( 'NONE',  ( -9.934419958767060521, 21.32062905558055022, -18.50213348364253818 ) ) ;
#11403 = DIRECTION ( 'NONE',  ( 1.000000000000000000, -0.000000000000000000, -0.000000000000000000 ) ) ;
#11404 = CARTESIAN_POINT ( 'NONE',  ( 36.57500000054621125, 13.80429023900056684, 86.29171490190961435 ) ) ;
#11405 = CARTESIAN_POINT ( 'NONE',  ( 22.77500000054622831, 20.00000000000000355, 83.50966788445364841 ) ) ;
#11406 = CARTESIAN_POINT ( 'NONE',  ( 10.00000000000001599, 19.48622803733975672, 98.29316153445364534 ) ) ;
#11407 = PLANE ( 'NONE',  #2579 ) ;
#11408 = EDGE_CURVE ( 'NONE', #5738, #8904, #4822, .T. ) ;
#11409 = AXIS2_PLACEMENT_3D ( 'NONE', #3143, #11651, #2959 ) ;
#11410 = CARTESIAN_POINT ( 'NONE',  ( -3.594513446512490388E-16, 55.00000000000000000, -21.00000000000000000 ) ) ;
#11411 = CARTESIAN_POINT ( 'NONE',  ( 92.00000000000000000, 6.757601037695094579E-16, -5.035999999999999588 ) ) ;
#11412 = CARTESIAN_POINT ( 'NONE',  ( 49.99999999999998579, 20.00000000000000355, 90.79316153445363113 ) ) ;
#11413 = ORIENTED_EDGE ( 'NONE', *, *, #498, .T. ) ;
#11414 = ADVANCED_BREP_SHAPE_REPRESENTATION ( '', ( #10428, #9021 ), #6962 ) ;
#11415 = FACE_OUTER_BOUND ( 'NONE', #10920, .T. ) ;
#11416 = EDGE_CURVE ( 'NONE', #2444, #11587, #4653, .T. ) ;
#11417 = DIRECTION ( 'NONE',  ( 0.000000000000000000, -0.07522014758255014810, 0.9971669516172604331 ) ) ;
#11418 = CIRCLE ( 'NONE', #5950, 5.999999999999998224 ) ;
#11419 = CARTESIAN_POINT ( 'NONE',  ( 24.67500000054622689, 15.71886984736413773, 84.90069139318163138 ) ) ;
#11420 = DIRECTION ( 'NONE',  ( -1.000000000000000000, -0.000000000000000000, -0.000000000000000000 ) ) ;
#11421 = AXIS2_PLACEMENT_3D ( 'NONE', #4627, #7423, #11226 ) ;
#11422 = CARTESIAN_POINT ( 'NONE',  ( 38.17500000054622689, 13.07298590277314254, 93.04388485072563242 ) ) ;
#11423 = EDGE_CURVE ( 'NONE', #724, #7452, #2317, .T. ) ;
#11424 = CARTESIAN_POINT ( 'NONE',  ( 25.37500000054622618, 27.65831843345427998, 90.79316153445363113 ) ) ;
#11425 = CARTESIAN_POINT ( 'NONE',  ( 30.29999999999998295, 13.62011893735971135, 95.42841645007781892 ) ) ;
#11426 = CARTESIAN_POINT ( 'NONE',  ( 38.57500000054622546, 15.71886984736413773, 84.90069139318163138 ) ) ;
#11427 = VERTEX_POINT ( 'NONE', #6432 ) ;
#11428 = CARTESIAN_POINT ( 'NONE',  ( 19.85000000109246443, 15.59161060780645691, 96.86078899226572503 ) ) ;
#11429 = DIRECTION ( 'NONE',  ( -1.000000000000000000, -0.000000000000000000, -0.000000000000000000 ) ) ;
#11430 = VERTEX_POINT ( 'NONE', #4781 ) ;
#11431 = CARTESIAN_POINT ( 'NONE',  ( 5.000000000000000000, 50.33115875943847328, 27.54995462791182348 ) ) ;
#11432 = VERTEX_POINT ( 'NONE', #845 ) ;
#11433 = CARTESIAN_POINT ( 'NONE',  ( 0.000000000000000000, 0.000000000000000000, 0.000000000000000000 ) ) ;
#11434 = CARTESIAN_POINT ( 'NONE',  ( 49.87500000054622262, 20.00000000000000355, 98.07665518445361386 ) ) ;
#11435 = DIRECTION ( 'NONE',  ( 0.000000000000000000, -1.039664082171044481E-15, -1.000000000000000000 ) ) ;
#11436 = CARTESIAN_POINT ( 'NONE',  ( 45.97500000054622404, 17.63344945572769973, 98.07665518445361386 ) ) ;
#11437 = CARTESIAN_POINT ( 'NONE',  ( 23.65000000109246514, 20.00000000000000355, 98.29316153445363113 ) ) ;
#11438 = CARTESIAN_POINT ( 'NONE',  ( 43.17500000054621978, 26.19570976099943493, 86.29171490190961435 ) ) ;
#11439 = CARTESIAN_POINT ( 'NONE',  ( 20.97500000054622404, 22.36655054427230382, 83.50966788445364841 ) ) ;
#11440 = VECTOR ( 'NONE', #4644, 1000.000000000000000 ) ;
#11441 = CARTESIAN_POINT ( 'NONE',  ( 41.19999999999998863, 24.40838939219355197, 84.72553407664153724 ) ) ;
#11442 = CARTESIAN_POINT ( 'NONE',  ( -5.000000000000004441, 0.000000000000000000, 69.99999999999998579 ) ) ;
#11443 = ORIENTED_EDGE ( 'NONE', *, *, #8936, .F. ) ;
#11444 = CARTESIAN_POINT ( 'NONE',  ( 35.25000000109245946, 27.13292387221364876, 93.11078899226573924 ) ) ;
#11445 = CARTESIAN_POINT ( 'NONE',  ( -50.00000000000001421, 31.99999999999960565, 124.8533255156881694 ) ) ;
#11446 = ORIENTED_EDGE ( 'NONE', *, *, #8225, .T. ) ;
#11447 = ORIENTED_EDGE ( 'NONE', *, *, #3831, .T. ) ;
#11448 = EDGE_CURVE ( 'NONE', #3939, #1799, #8196, .T. ) ;
#11449 = CARTESIAN_POINT ( 'NONE',  ( -7.946065455725393356, 26.10639172058064972, -23.70672747870507280 ) ) ;
#11450 = VECTOR ( 'NONE', #12421, 1000.000000000000227 ) ;
#11451 = CARTESIAN_POINT ( 'NONE',  ( 5.854672968065819383, 11.88659906342193295, -20.16928711762458448 ) ) ;
#11452 = CARTESIAN_POINT ( 'NONE',  ( -1.651830483015944262, 29.86811216670179903, 24.94746627493933744 ) ) ;
#11453 = VECTOR ( 'NONE', #10449, 999.9999999999998863 ) ;
#11454 = CARTESIAN_POINT ( 'NONE',  ( 10.00000000000000178, 0.000000000000000000, 0.000000000000000000 ) ) ;
#11455 = CARTESIAN_POINT ( 'NONE',  ( -4.336320944401498956, 47.48960973344409098, 20.54824459866649988 ) ) ;
#11456 = ORIENTED_EDGE ( 'NONE', *, *, #3248, .T. ) ;
#11457 = CARTESIAN_POINT ( 'NONE',  ( 2.507195821380045153, 54.33828039948598843, -27.88885893167862662 ) ) ;
#11458 = CARTESIAN_POINT ( 'NONE',  ( 0.000000000000000000, 50.00000000000000000, -28.00000000000000711 ) ) ;
#11459 = CARTESIAN_POINT ( 'NONE',  ( 22.47500000054623115, 13.80429023900056684, 86.29171490190961435 ) ) ;
#11460 = CARTESIAN_POINT ( 'NONE',  ( 12.00000000000000355, 0.000000000000000000, 9.000000000000000000 ) ) ;
#11461 = DIRECTION ( 'NONE',  ( 0.000000000000000000, 0.000000000000000000, -1.000000000000000000 ) ) ;
#11462 = ORIENTED_EDGE ( 'NONE', *, *, #11101, .T. ) ;
#11463 = DIRECTION ( 'NONE',  ( 0.000000000000000000, 1.000000000000000000, -1.039664082171044875E-15 ) ) ;
#11464 = CARTESIAN_POINT ( 'NONE',  ( 21.29999999999999005, 26.37988106264029398, 86.15790661882942914 ) ) ;
#11465 = EDGE_CURVE ( 'NONE', #9270, #5416, #692, .T. ) ;
#11466 = CARTESIAN_POINT ( 'NONE',  ( -31.74999999999995737, 0.000000000000000000, 0.000000000000000000 ) ) ;
#11467 = CARTESIAN_POINT ( 'NONE',  ( 20.27500000054622831, 12.34168156654572357, 90.79316153445363113 ) ) ;
#11468 = DIRECTION ( 'NONE',  ( -1.000000000000000000, -0.000000000000000000, -0.000000000000000000 ) ) ;
#11469 = EDGE_CURVE ( 'NONE', #7687, #5616, #3632, .T. ) ;
#11470 = CARTESIAN_POINT ( 'NONE',  ( -4.735706364529653989, 51.61244378856764570, -20.45911749698736060 ) ) ;
#11471 = CARTESIAN_POINT ( 'NONE',  ( 49.99999999999998579, 22.00000000000000000, 69.99999999999998579 ) ) ;
#11472 = CARTESIAN_POINT ( 'NONE',  ( 5.000000000000000000, 49.66912405214284831, 27.54995462791181637 ) ) ;
#11473 = DIRECTION ( 'NONE',  ( 1.000000000000000000, -0.000000000000000000, -0.000000000000000000 ) ) ;
#11474 = ORIENTED_EDGE ( 'NONE', *, *, #8993, .F. ) ;
#11475 = DIRECTION ( 'NONE',  ( -1.000000000000000000, 0.000000000000000000, 0.000000000000000000 ) ) ;
#11476 = DIRECTION ( 'NONE',  ( 1.000000000000000000, 0.000000000000000000, 0.000000000000000000 ) ) ;
#11477 = AXIS2_PLACEMENT_3D ( 'NONE', #11911, #4099, #4234 ) ;
#11478 = CARTESIAN_POINT ( 'NONE',  ( 29.35000000109245732, 26.37988106264029398, 95.42841645007781892 ) ) ;
#11479 = CARTESIAN_POINT ( 'NONE',  ( 41.47500000054623115, 26.19570976099943849, 95.29460816699764791 ) ) ;
#11480 = CARTESIAN_POINT ( 'NONE',  ( 28.07500000054622546, 15.71886984736413417, 96.68563167572563088 ) ) ;
#11481 = CARTESIAN_POINT ( 'NONE',  ( 26.79999999999998650, 15.59161060780646046, 84.72553407664153724 ) ) ;
#11482 = ADVANCED_FACE ( 'NONE', ( #2750 ), #2512, .F. ) ;
#11483 = DIRECTION ( 'NONE',  ( -0.000000000000000000, -0.000000000000000000, 1.000000000000000000 ) ) ;
#11484 = CARTESIAN_POINT ( 'NONE',  ( 31.17500000054622689, 26.92701409722686634, 88.54243821818162985 ) ) ;
#11485 = ORIENTED_EDGE ( 'NONE', *, *, #9369, .F. ) ;
#11486 = CARTESIAN_POINT ( 'NONE',  ( 49.47500000054621694, 26.19570976099943493, 95.29460816699764791 ) ) ;
#11487 = CARTESIAN_POINT ( 'NONE',  ( -0.3269246974466745170, 45.00000000000000000, -20.99999999999999289 ) ) ;
#11488 = CIRCLE ( 'NONE', #1369, 9.499999999999994671 ) ;
#11489 = ORIENTED_EDGE ( 'NONE', *, *, #10572, .F. ) ;
#11490 = CARTESIAN_POINT ( 'NONE',  ( 10.00000000000000355, 20.00000000000000355, 18.46618531261938401 ) ) ;
#11491 = ORIENTED_EDGE ( 'NONE', *, *, #3025, .F. ) ;
#11492 = ADVANCED_FACE ( 'NONE', ( #6552 ), #8584, .F. ) ;
#11493 = CARTESIAN_POINT ( 'NONE',  ( 42.45000000109246940, 15.59161060780646046, 84.72553407664153724 ) ) ;
#11494 = DIRECTION ( 'NONE',  ( 1.000000000000000000, 0.000000000000000000, 0.000000000000000000 ) ) ;
#11495 = CARTESIAN_POINT ( 'NONE',  ( 6.000000000000000000, 6.193651186687738874E-16, -5.057500000000000107 ) ) ;
#11496 = CARTESIAN_POINT ( 'NONE',  ( 41.67500000054622689, 24.28113015263587116, 96.68563167572563088 ) ) ;
#11497 = CARTESIAN_POINT ( 'NONE',  ( 20.99999999999998579, 20.00000000000000355, 83.29316153445364534 ) ) ;
#11498 = AXIS2_PLACEMENT_3D ( 'NONE', #8579, #11435, #12390 ) ;
#11499 = SURFACE_STYLE_FILL_AREA ( #6732 ) ;
#11500 = CARTESIAN_POINT ( 'NONE',  ( 42.77500000054622831, 17.63344945572770328, 83.50966788445364841 ) ) ;
#11501 = CARTESIAN_POINT ( 'NONE',  ( 48.69999999999998153, 13.62011893735971135, 86.15790661882942914 ) ) ;
#11502 = CARTESIAN_POINT ( 'NONE',  ( -5.845037936402837531, 28.12045204670673826, -24.30869324251348829 ) ) ;
#11503 = PLANE ( 'NONE',  #5441 ) ;
#11504 = ORIENTED_EDGE ( 'NONE', *, *, #12481, .T. ) ;
#11505 = CARTESIAN_POINT ( 'NONE',  ( 40.55000000109247082, 17.56310227825321135, 83.29316153445363113 ) ) ;
#11506 = ORIENTED_EDGE ( 'NONE', *, *, #8095, .T. ) ;
#11507 = DIRECTION ( 'NONE',  ( 0.000000000000000000, 0.000000000000000000, -1.000000000000000000 ) ) ;
#11508 = ORIENTED_EDGE ( 'NONE', *, *, #3401, .F. ) ;
#11509 = FACE_OUTER_BOUND ( 'NONE', #1231, .T. ) ;
#11510 = CARTESIAN_POINT ( 'NONE',  ( 2.631235708468342871, 10.32974564483150814, -20.84467326578077362 ) ) ;
#11511 = CARTESIAN_POINT ( 'NONE',  ( -8.483825669166648709, 25.30371668182424827, 23.51725424962153355 ) ) ;
#11512 =( BOUNDED_CURVE ( )  B_SPLINE_CURVE ( 2, ( #12374, #3674, #1767, #11478, #8564, #7551, #2601, #9339, #10519, #12310, #3733 ),
 .UNSPECIFIED., .F., .F. ) 
 B_SPLINE_CURVE_WITH_KNOTS ( ( 3, 2, 2, 2, 2, 3 ),
 ( 0.6666666666666666297, 0.6733333333333333393, 0.6800000000000000488, 0.6866666666666666474, 0.6933333333333333570, 0.6999999999999999556 ),
 .UNSPECIFIED. ) 
 CURVE ( )  GEOMETRIC_REPRESENTATION_ITEM ( )  RATIONAL_B_SPLINE_CURVE ( ( 1.000000000000000000, 0.9510565162951535312, 1.000000000000000000, 0.9510565162951535312, 1.000000000000000000, 0.9510565162951535312, 1.000000000000000000, 0.9510565162951535312, 1.000000000000000000, 0.9510565162951535312, 1.000000000000000000 ) ) 
 REPRESENTATION_ITEM ( '' )  );
#11513 = VECTOR ( 'NONE', #4874, 1000.000000000000000 ) ;
#11514 = LINE ( 'NONE', #11335, #517 ) ;
#11515 = CARTESIAN_POINT ( 'NONE',  ( 22.09999999999998366, 17.56310227825320425, 98.29316153445363113 ) ) ;
#11516 = VERTEX_POINT ( 'NONE', #5611 ) ;
#11517 = CARTESIAN_POINT ( 'NONE',  ( -31.74999999999995737, 0.000000000000000000, 6.000000000000000000 ) ) ;
#11518 = CARTESIAN_POINT ( 'NONE',  ( 48.65000000109246514, 20.00000000000000355, 83.29316153445364534 ) ) ;
#11519 = CARTESIAN_POINT ( 'NONE',  ( 22.27500000054622475, 12.34168156654572535, 90.79316153445363113 ) ) ;
#11520 = ORIENTED_EDGE ( 'NONE', *, *, #8701, .T. ) ;
#11521 = CARTESIAN_POINT ( 'NONE',  ( -20.27158385259951956, 22.00000000000000000, 152.2284161474004520 ) ) ;
#11522 = CARTESIAN_POINT ( 'NONE',  ( -28.50000000000001066, 77.00000000000000000, 104.8533255156881836 ) ) ;
#11523 = EDGE_LOOP ( 'NONE', ( #8590, #278 ) ) ;
#11524 = COLOUR_RGB ( '',0.7921568627450980005, 0.8196078431372548767, 0.9333333333333333481 ) ;
#11525 =( REPRESENTATION_RELATIONSHIP ('NONE','NONE', #4262, #10013 ) REPRESENTATION_RELATIONSHIP_WITH_TRANSFORMATION ( #11860 )SHAPE_REPRESENTATION_RELATIONSHIP( ) );
#11526 = ORIENTED_EDGE ( 'NONE', *, *, #5526, .F. ) ;
#11527 = CLOSED_SHELL ( 'NONE', ( #7541, #6912, #8785, #11864, #4982, #2710, #11924, #10176, #10157, #5744, #12110, #3735, #10258, #4914, #8275, #9638, #8553, #333 ) ) ;
#11528 = CARTESIAN_POINT ( 'NONE',  ( 42.85000000109246798, 24.40838939219355197, 84.72553407664153724 ) ) ;
#11529 = FACE_OUTER_BOUND ( 'NONE', #1111, .T. ) ;
#11530 = CARTESIAN_POINT ( 'NONE',  ( 21.57500000054622546, 24.28113015263587116, 96.68563167572563088 ) ) ;
#11531 = EDGE_CURVE ( 'NONE', #6613, #1932, #2493, .T. ) ;
#11532 = VECTOR ( 'NONE', #12118, 1000.000000000000000 ) ;
#11533 = CARTESIAN_POINT ( 'NONE',  ( 10.00000000000000355, 20.00000000000000355, 98.29316153445363113 ) ) ;
#11534 = CYLINDRICAL_SURFACE ( 'NONE', #7787, 7.500000000000000000 ) ;
#11535 = CARTESIAN_POINT ( 'NONE',  ( -6.500000000000214051, 40.00000000000000000, 26.49999999999998934 ) ) ;
#11536 = CARTESIAN_POINT ( 'NONE',  ( -20.27158385259951956, 22.00000000000000000, 170.0000119999999697 ) ) ;
#11537 = VECTOR ( 'NONE', #8396, 1000.000000000000000 ) ;
#11538 = DIRECTION ( 'NONE',  ( 0.000000000000000000, 0.000000000000000000, -1.000000000000000000 ) ) ;
#11539 = EDGE_LOOP ( 'NONE', ( #2548, #9908, #3142, #8016 ) ) ;
#11540 = CARTESIAN_POINT ( 'NONE',  ( -5.023203578122774182, 11.34694221345378828, -27.54729890636757261 ) ) ;
#11541 = APPLICATION_PROTOCOL_DEFINITION ( 'draft international standard', 'automotive_design', 1998, #7562 ) ;
#11542 = CARTESIAN_POINT ( 'NONE',  ( 26.07500000054622546, 15.71886984736413417, 96.68563167572563088 ) ) ;
#11543 = DIRECTION ( 'NONE',  ( 0.000000000000000000, -1.224646799147353207E-16, 1.000000000000000000 ) ) ;
#11544 = CARTESIAN_POINT ( 'NONE',  ( 42.07500000054623257, 13.80429023900056507, 95.29460816699764791 ) ) ;
#11545 = CARTESIAN_POINT ( 'NONE',  ( 25.97500000054622049, 17.63344945572769973, 98.07665518445361386 ) ) ;
#11546 = CARTESIAN_POINT ( 'NONE',  ( 29.29999999999998650, 26.37988106264029398, 86.15790661882942914 ) ) ;
#11547 = CARTESIAN_POINT ( 'NONE',  ( 49.99999999999998579, 18.00000000000000355, 152.2284161474004520 ) ) ;
#11548 = CARTESIAN_POINT ( 'NONE',  ( 32.07500000054623257, 13.80429023900056507, 95.29460816699764791 ) ) ;
#11549 = EDGE_LOOP ( 'NONE', ( #7956, #6942, #5497 ) ) ;
#11550 = CIRCLE ( 'NONE', #413, 0.5999999999999998668 ) ;
#11551 = PRODUCT_DEFINITION_SHAPE ( 'NONE', 'NONE',  #12553 ) ;
#11552 = EDGE_CURVE ( 'NONE', #12402, #7152, #2999, .T. ) ;
#11553 = DIRECTION ( 'NONE',  ( 0.000000000000000000, 1.000000000000000000, 0.000000000000000000 ) ) ;
#11554 = ORIENTED_EDGE ( 'NONE', *, *, #5968, .T. ) ;
#11555 = CARTESIAN_POINT ( 'NONE',  ( -9.105758978599869380, 24.14626203848898101, -26.47834574479485070 ) ) ;
#11556 = ORIENTED_EDGE ( 'NONE', *, *, #3765, .T. ) ;
#11557 = CARTESIAN_POINT ( 'NONE',  ( 49.99999999999998579, 20.00000000000000000, 145.0000000000000000 ) ) ;
#11558 = CARTESIAN_POINT ( 'NONE',  ( -34.99999999999997868, 20.00000000000000000, 137.5000000000000000 ) ) ;
#11559 = FACE_OUTER_BOUND ( 'NONE', #5772, .T. ) ;
#11560 = AXIS2_PLACEMENT_3D ( 'NONE', #3363, #1408, #5274 ) ;
#11561 = DIRECTION ( 'NONE',  ( 0.000000000000000000, 0.000000000000000000, 1.000000000000000000 ) ) ;
#11562 = DIRECTION ( 'NONE',  ( -1.000000000000000000, -0.000000000000000000, -0.000000000000000000 ) ) ;
#11563 = CARTESIAN_POINT ( 'NONE',  ( 47.07500000054622546, 24.28113015263587471, 84.90069139318163138 ) ) ;
#11564 = CARTESIAN_POINT ( 'NONE',  ( 49.89999999999998437, 22.43689772174679575, 98.29316153445363113 ) ) ;
#11565 = DIRECTION ( 'NONE',  ( -0.000000000000000000, 1.000000000000000000, -0.000000000000000000 ) ) ;
#11566 = CARTESIAN_POINT ( 'NONE',  ( 49.17500000054622689, 26.92701409722686634, 88.54243821818162985 ) ) ;
#11567 = ORIENTED_EDGE ( 'NONE', *, *, #6998, .F. ) ;
#11568 = EDGE_CURVE ( 'NONE', #6113, #10800, #90, .T. ) ;
#11569 = CARTESIAN_POINT ( 'NONE',  ( 34.25000000109245946, 12.86707612778636012, 88.47553407664152303 ) ) ;
#11570 = ORIENTED_EDGE ( 'NONE', *, *, #11969, .F. ) ;
#11571 =( NAMED_UNIT ( * ) PLANE_ANGLE_UNIT ( ) SI_UNIT ( $, .RADIAN. ) );
#11572 = AXIS2_PLACEMENT_3D ( 'NONE', #1425, #12077, #4456 ) ;
#11573 = ORIENTED_EDGE ( 'NONE', *, *, #3207, .T. ) ;
#11574 = B_SPLINE_CURVE_WITH_KNOTS ( 'NONE', 3,
 ( #3343, #8357, #10076, #10252, #7336, #10139, #7211, #8236, #12224, #3404, #3526, #8418, #11145, #1628, #4297, #1506, #7399, #11270, #4418, #2575, #1450, #6447, #9375, #12288, #2335, #6204 ),
 .UNSPECIFIED., .F., .F.,
 ( 4, 2, 2, 2, 2, 2, 2, 2, 2, 2, 2, 2, 4 ),
 ( 0.01588129651937168763, 0.01687311342740074882, 0.01786493033542981002, 0.01885674724345887468, 0.01984856415148793934, 0.02183219796754606173, 0.02381583178360418412, 0.02579946559966230998, 0.02679128250769137465, 0.02778309941572043584, 0.02877491632374950398, 0.02976673323177856517, 0.03175036704783668062 ),
 .UNSPECIFIED. ) ;
#11575 = DIRECTION ( 'NONE',  ( -0.000000000000000000, -0.000000000000000000, 1.000000000000000000 ) ) ;
#11576 = EDGE_CURVE ( 'NONE', #9005, #3772, #7822, .T. ) ;
#11577 = CARTESIAN_POINT ( 'NONE',  ( 9.102720968516898381, 15.84716940310434197, -18.92511261036585779 ) ) ;
#11578 = DIRECTION ( 'NONE',  ( 1.000000000000000000, 0.000000000000000000, 0.000000000000000000 ) ) ;
#11579 = CARTESIAN_POINT ( 'NONE',  ( 38.67500000054623399, 17.63344945572770328, 83.50966788445364841 ) ) ;
#11580 = DIRECTION ( 'NONE',  ( 0.000000000000000000, 0.000000000000000000, -1.000000000000000000 ) ) ;
#11581 = CARTESIAN_POINT ( 'NONE',  ( 0.6668850494917962779, 30.00000000000000355, -28.00000000000000711 ) ) ;
#11582 = CARTESIAN_POINT ( 'NONE',  ( 0.000000000000000000, 20.00000000000000355, -70.00000000000000000 ) ) ;
#11583 = ORIENTED_EDGE ( 'NONE', *, *, #4810, .T. ) ;
#11584 = CARTESIAN_POINT ( 'NONE',  ( 1.609999862365107504, 54.73655139282131898, -27.95411785540357030 ) ) ;
#11585 = DIRECTION ( 'NONE',  ( 0.000000000000000000, 0.000000000000000000, -1.000000000000000000 ) ) ;
#11586 = CARTESIAN_POINT ( 'NONE',  ( 48.17500000054622689, 13.80429023900056507, 95.29460816699764791 ) ) ;
#11587 = VERTEX_POINT ( 'NONE', #11755 ) ;
#11588 = CARTESIAN_POINT ( 'NONE',  ( 0.6000000000000033085, 0.000000000000000000, 0.000000000000000000 ) ) ;
#11589 = CARTESIAN_POINT ( 'NONE',  ( 2.509213302053919570, 54.33723024690351622, -20.85136804008542555 ) ) ;
#11590 = ORIENTED_EDGE ( 'NONE', *, *, #6688, .F. ) ;
#11591 = ORIENTED_EDGE ( 'NONE', *, *, #18, .T. ) ;
#11592 =( BOUNDED_CURVE ( )  B_SPLINE_CURVE ( 2, ( #1632, #742, #7531, #3409, #1573, #5386, #11208, #9257, #11398, #9440, #10313 ),
 .UNSPECIFIED., .F., .F. ) 
 B_SPLINE_CURVE_WITH_KNOTS ( ( 3, 2, 2, 2, 2, 3 ),
 ( 0.06666666666666672125, 0.07333333333333338921, 0.08000000000000007105, 0.08666666666666673902, 0.09333333333333342086, 0.1000000000000000888 ),
 .UNSPECIFIED. ) 
 CURVE ( )  GEOMETRIC_REPRESENTATION_ITEM ( )  RATIONAL_B_SPLINE_CURVE ( ( 0.9999999999999995559, 0.9510565162951539753, 1.000000000000000000, 0.9510565162951535312, 1.000000000000000000, 0.9510565162951535312, 1.000000000000000000, 0.9510565162951535312, 1.000000000000000000, 0.9510565162951529761, 1.000000000000000666 ) ) 
 REPRESENTATION_ITEM ( '' )  );
#11593 = CARTESIAN_POINT ( 'NONE',  ( 43.25000000109246656, 27.13292387221364876, 93.11078899226573924 ) ) ;
#11594 = CARTESIAN_POINT ( 'NONE',  ( -33.79382810696421302, 25.37779564132840804, 151.2938281069642130 ) ) ;
#11595 = FACE_OUTER_BOUND ( 'NONE', #2609, .T. ) ;
#11596 = CARTESIAN_POINT ( 'NONE',  ( 1.300123024442352504, 45.16070347875686508, -24.96827571664099565 ) ) ;
#11597 = FACE_OUTER_BOUND ( 'NONE', #11771, .T. ) ;
#11598 = CARTESIAN_POINT ( 'NONE',  ( 19.77500000054622831, 20.00000000000000355, 98.07665518445361386 ) ) ;
#11599 = CARTESIAN_POINT ( 'NONE',  ( 4.491735821183317157, 47.77958954773085765, 27.63766201934051026 ) ) ;
#11600 = CARTESIAN_POINT ( 'NONE',  ( 5.022951428105686844, 11.32827475346531720, 24.49655794125914099 ) ) ;
#11601 = ORIENTED_EDGE ( 'NONE', *, *, #12266, .F. ) ;
#11602 = CARTESIAN_POINT ( 'NONE',  ( 0.6684871184501431918, 29.98311267939276092, -24.99323153604321490 ) ) ;
#11603 = UNCERTAINTY_MEASURE_WITH_UNIT (LENGTH_MEASURE( 1.000000000000000082E-05 ), #5278, 'distance_accuracy_value', 'NONE');
#11604 = EDGE_CURVE ( 'NONE', #10983, #8716, #9606, .T. ) ;
#11605 = CARTESIAN_POINT ( 'NONE',  ( 28.17500000054621978, 13.80429023900056507, 95.29460816699764791 ) ) ;
#11606 = DIRECTION ( 'NONE',  ( 0.000000000000000000, 0.000000000000000000, -1.000000000000000000 ) ) ;
#11607 = CIRCLE ( 'NONE', #2075, 17.49999999999996803 ) ;
#11608 = EDGE_CURVE ( 'NONE', #7259, #6104, #152, .T. ) ;
#11609 = CARTESIAN_POINT ( 'NONE',  ( 38.37500000054622973, 13.07298590277314432, 88.54243821818161564 ) ) ;
#11610 = CARTESIAN_POINT ( 'NONE',  ( 30.67500000054622333, 15.71886984736413773, 84.90069139318163138 ) ) ;
#11611 = CARTESIAN_POINT ( 'NONE',  ( 23.59999999999999076, 27.13292387221364876, 93.11078899226573924 ) ) ;
#11612 = CARTESIAN_POINT ( 'NONE',  ( 34.39999999999998437, 12.86707612778636012, 93.11078899226572503 ) ) ;
#11613 = CARTESIAN_POINT ( 'NONE',  ( 33.37500000054622973, 26.92701409722686634, 93.04388485072563242 ) ) ;
#11614 = VERTEX_POINT ( 'NONE', #4073 ) ;
#11615 = FACE_OUTER_BOUND ( 'NONE', #4407, .T. ) ;
#11616 = ORIENTED_EDGE ( 'NONE', *, *, #1352, .T. ) ;
#11617 = LINE ( 'NONE', #1092, #4067 ) ;
#11618 = ORIENTED_EDGE ( 'NONE', *, *, #5454, .T. ) ;
#11619 = AXIS2_PLACEMENT_3D ( 'NONE', #4484, #7400, #9317 ) ;
#11620 =( NAMED_UNIT ( * ) PLANE_ANGLE_UNIT ( ) SI_UNIT ( $, .RADIAN. ) );
#11621 = FACE_OUTER_BOUND ( 'NONE', #1941, .T. ) ;
#11622 = AXIS2_PLACEMENT_3D ( 'NONE', #8433, #2406, #2465 ) ;
#11623 = DIRECTION ( 'NONE',  ( -0.000000000000000000, -0.000000000000000000, -1.000000000000000000 ) ) ;
#11624 = CARTESIAN_POINT ( 'NONE',  ( 42.97500000054622404, 22.36655054427230382, 83.50966788445364841 ) ) ;
#11625 = CARTESIAN_POINT ( 'NONE',  ( -2.000000000000015543, 20.00000000000000355, 90.79316153445363113 ) ) ;
#11626 = EDGE_CURVE ( 'NONE', #5275, #4582, #4131, .T. ) ;
#11627 = SURFACE_SIDE_STYLE ('',( #11499 ) ) ;
#11628 = CARTESIAN_POINT ( 'NONE',  ( 45.57500000054621836, 26.19570976099943493, 95.29460816699764791 ) ) ;
#11629 = CARTESIAN_POINT ( 'NONE',  ( 46.69999999999998153, 13.62011893735971135, 86.15790661882942914 ) ) ;
#11630 = AXIS2_PLACEMENT_3D ( 'NONE', #6428, #9232, #7189 ) ;
#11631 = CARTESIAN_POINT ( 'NONE',  ( 45.69999999999998863, 26.37988106264029398, 95.42841645007781892 ) ) ;
#11632 = DIRECTION ( 'NONE',  ( 1.000000000000000000, 0.000000000000000000, 0.000000000000000000 ) ) ;
#11633 = ORIENTED_EDGE ( 'NONE', *, *, #5095, .F. ) ;
#11634 = AXIS2_PLACEMENT_3D ( 'NONE', #1886, #9452, #1757 ) ;
#11635 = EDGE_CURVE ( 'NONE', #2031, #7888, #3451, .T. ) ;
#11636 = CARTESIAN_POINT ( 'NONE',  ( 32.35000000109246088, 13.62011893735971135, 86.15790661882942914 ) ) ;
#11637 = DIRECTION ( 'NONE',  ( -1.000000000000000000, -0.000000000000000000, -0.000000000000000000 ) ) ;
#11638 = ORIENTED_EDGE ( 'NONE', *, *, #796, .T. ) ;
#11639 = ORIENTED_EDGE ( 'NONE', *, *, #3769, .T. ) ;
#11640 = DIRECTION ( 'NONE',  ( -1.000000000000000000, 0.000000000000000000, 0.000000000000000000 ) ) ;
#11641 = DIRECTION ( 'NONE',  ( -0.7071067811865500152, 8.659560562354962440E-17, 0.7071067811865451302 ) ) ;
#11642 = VECTOR ( 'NONE', #470, 1000.000000000000000 ) ;
#11643 = CARTESIAN_POINT ( 'NONE',  ( 47.99999999999998579, 20.00000000000000355, 98.29316153445363113 ) ) ;
#11644 = CARTESIAN_POINT ( 'NONE',  ( 34.57500000054623257, 15.71886984736413773, 84.90069139318163138 ) ) ;
#11645 = CARTESIAN_POINT ( 'NONE',  ( 40.97500000054622404, 22.36655054427230382, 83.50966788445364841 ) ) ;
#11646 = CARTESIAN_POINT ( 'NONE',  ( -0.3267839603878587851, 54.99999999999999289, 28.00000000000000355 ) ) ;
#11647 = DIRECTION ( 'NONE',  ( -1.000000000000000000, -0.000000000000000000, -0.000000000000000000 ) ) ;
#11648 = CARTESIAN_POINT ( 'NONE',  ( 32.00000000000000000, 0.000000000000000000, 0.000000000000000000 ) ) ;
#11649 = ORIENTED_EDGE ( 'NONE', *, *, #5104, .T. ) ;
#11650 = EDGE_CURVE ( 'NONE', #8904, #9005, #777, .T. ) ;
#11651 = DIRECTION ( 'NONE',  ( 0.000000000000000000, 0.000000000000000000, -1.000000000000000000 ) ) ;
#11652 = EDGE_LOOP ( 'NONE', ( #6872, #9020, #654, #10855 ) ) ;
#11653 = CARTESIAN_POINT ( 'NONE',  ( 3.061616998149962604E-15, 10.00000000000000000, 25.00000000000000000 ) ) ;
#11654 = AXIS2_PLACEMENT_3D ( 'NONE', #5564, #6566, #7712 ) ;
#11655 = UNCERTAINTY_MEASURE_WITH_UNIT (LENGTH_MEASURE( 1.000000000000000082E-05 ), #362, 'distance_accuracy_value', 'NONE');
#11656 = CARTESIAN_POINT ( 'NONE',  ( 6.000000000000000000, -2.919948986426525117, 5.057500000000004547 ) ) ;
#11657 = ORIENTED_EDGE ( 'NONE', *, *, #7312, .F. ) ;
#11658 = ORIENTED_EDGE ( 'NONE', *, *, #139, .F. ) ;
#11659 = EDGE_CURVE ( 'NONE', #7797, #6710, #8311, .T. ) ;
#11660 = CARTESIAN_POINT ( 'NONE',  ( -6.117437525492237960, 27.91716672128773880, -20.09092915124056233 ) ) ;
#11661 = DIRECTION ( 'NONE',  ( -0.000000000000000000, -1.000000000000000000, -0.000000000000000000 ) ) ;
#11662 = VECTOR ( 'NONE', #3188, 1000.000000000000000 ) ;
#11663 = CARTESIAN_POINT ( 'NONE',  ( 7.615685201709251118, 26.48948478036892595, 94.58229401248311774 ) ) ;
#11664 = CARTESIAN_POINT ( 'NONE',  ( 4.491542451266983704, 47.77873343313099497, -24.59354576118897739 ) ) ;
#11665 = DIRECTION ( 'NONE',  ( 1.000000000000000000, 0.000000000000000000, -0.000000000000000000 ) ) ;
#11666 = CARTESIAN_POINT ( 'NONE',  ( -6.999999999999999112, 92.00000000000000000, 166.8533255156881694 ) ) ;
#11667 = CARTESIAN_POINT ( 'NONE',  ( 4.967476492172508529, 49.34237399800478840, 27.55591537130747426 ) ) ;
#11668 = VECTOR ( 'NONE', #8175, 1000.000000000000000 ) ;
#11669 = DIRECTION ( 'NONE',  ( -1.000000000000000000, 0.000000000000000000, 0.000000000000000000 ) ) ;
#11670 = ORIENTED_EDGE ( 'NONE', *, *, #5505, .T. ) ;
#11671 = CARTESIAN_POINT ( 'NONE',  ( 9.739799295956466096, 22.29052955100696920, -23.02479834983350671 ) ) ;
#11672 = CIRCLE ( 'NONE', #6201, 9.000000000000000000 ) ;
#11673 = ITEM_DEFINED_TRANSFORMATION ( 'NONE', 'NONE', #6764,  #9021 ) ;
#11674 = CARTESIAN_POINT ( 'NONE',  ( 22.47500000054622404, 13.07298590277314432, 88.54243821818161564 ) ) ;
#11675 = CARTESIAN_POINT ( 'NONE',  ( 48.77500000054623541, 17.63344945572770328, 83.50966788445364841 ) ) ;
#11676 = CARTESIAN_POINT ( 'NONE',  ( 38.57500000054622546, 15.71886984736413773, 84.90069139318163138 ) ) ;
#11677 = CARTESIAN_POINT ( 'NONE',  ( 20.37500000054621907, 12.34168156654572535, 90.79316153445363113 ) ) ;
#11678 = CARTESIAN_POINT ( 'NONE',  ( 22.39999999999998437, 12.86707612778636012, 93.11078899226572503 ) ) ;
#11679 =( LENGTH_UNIT ( ) NAMED_UNIT ( * ) SI_UNIT ( .MILLI., .METRE. ) );
#11680 = CARTESIAN_POINT ( 'NONE',  ( 31.37500000054622973, 26.92701409722686634, 93.04388485072563242 ) ) ;
#11681 = ORIENTED_EDGE ( 'NONE', *, *, #2280, .T. ) ;
#11682 = CYLINDRICAL_SURFACE ( 'NONE', #2432, 25.00000000000000000 ) ;
#11683 = ORIENTED_EDGE ( 'NONE', *, *, #4944, .T. ) ;
#11684 = LINE ( 'NONE', #4958, #7314 ) ;
#11685 = ORIENTED_EDGE ( 'NONE', *, *, #11811, .T. ) ;
#11686 = DIRECTION ( 'NONE',  ( -0.000000000000000000, -0.000000000000000000, 1.000000000000000000 ) ) ;
#11687 = CYLINDRICAL_SURFACE ( 'NONE', #3571, 7.500000000000000000 ) ;
#11688 = CARTESIAN_POINT ( 'NONE',  ( 38.77500000054622831, 17.63344945572770328, 83.50966788445364841 ) ) ;
#11689 = FACE_OUTER_BOUND ( 'NONE', #11011, .T. ) ;
#11690 = CARTESIAN_POINT ( 'NONE',  ( 44.29999999999999716, 13.62011893735971135, 95.42841645007781892 ) ) ;
#11691 = PRESENTATION_LAYER_ASSIGNMENT (  '', '', ( #5415 ) ) ;
#11692 = CARTESIAN_POINT ( 'NONE',  ( -50.00000000000001421, 92.00000000000000000, 69.99999999999998579 ) ) ;
#11693 = ADVANCED_FACE ( 'NONE', ( #6281 ), #6401, .F. ) ;
#11694 = FACE_OUTER_BOUND ( 'NONE', #1511, .T. ) ;
#11695 = VERTEX_POINT ( 'NONE', #1642 ) ;
#11696 = CARTESIAN_POINT ( 'NONE',  ( 30.55000000109246372, 17.56310227825321135, 83.29316153445363113 ) ) ;
#11697 = CARTESIAN_POINT ( 'NONE',  ( 0.3267965066156393039, 44.99999999999999289, -25.00000000000000355 ) ) ;
#11698 = VERTEX_POINT ( 'NONE', #3543 ) ;
#11699 = ADVANCED_FACE ( 'NONE', ( #7479 ), #7416, .F. ) ;
#11700 = ORIENTED_EDGE ( 'NONE', *, *, #7126, .T. ) ;
#11701 = CARTESIAN_POINT ( 'NONE',  ( -1.324565580760808992, 29.93364609169914914, -24.97324923543901320 ) ) ;
#11702 = AXIS2_PLACEMENT_3D ( 'NONE', #6309, #9230, #12018 ) ;
#11703 = LINE ( 'NONE', #9867, #9677 ) ;
#11704 = CARTESIAN_POINT ( 'NONE',  ( 48.29999999999999005, 13.62011893735970958, 95.42841645007781892 ) ) ;
#11705 = ADVANCED_FACE ( 'NONE', ( #2658 ), #9391, .F. ) ;
#11706 = CARTESIAN_POINT ( 'NONE',  ( 37.67500000054623399, 22.36655054427230027, 98.07665518445361386 ) ) ;
#11707 = CARTESIAN_POINT ( 'NONE',  ( 32.87500000054622262, 20.00000000000000355, 83.50966788445364841 ) ) ;
#11708 = CARTESIAN_POINT ( 'NONE',  ( 44.45000000109246230, 15.59161060780646046, 84.72553407664153724 ) ) ;
#11709 = CYLINDRICAL_SURFACE ( 'NONE', #774, 7.499999999999992895 ) ;
#11710 = ORIENTED_EDGE ( 'NONE', *, *, #490, .T. ) ;
#11711 = CARTESIAN_POINT ( 'NONE',  ( 48.55000000109246372, 17.56310227825321135, 83.29316153445363113 ) ) ;
#11712 = CARTESIAN_POINT ( 'NONE',  ( -6.999999999999999112, 55.00000000000000000, 147.8533255156883399 ) ) ;
#11713 = ORIENTED_EDGE ( 'NONE', *, *, #4489, .T. ) ;
#11714 = FACE_OUTER_BOUND ( 'NONE', #10853, .T. ) ;
#11715 =( BOUNDED_CURVE ( )  B_SPLINE_CURVE ( 2, ( #5668, #12264, #11493, #6602, #3812, #5604, #837, #12448, #2617, #7630, #655 ),
 .UNSPECIFIED., .F., .F. ) 
 B_SPLINE_CURVE_WITH_KNOTS ( ( 3, 2, 2, 2, 2, 3 ),
 ( 0.2333333333333333093, 0.2399999999999999634, 0.2466666666666666452, 0.2533333333333333548, 0.2600000000000000089, 0.2666666666666666630 ),
 .UNSPECIFIED. ) 
 CURVE ( )  GEOMETRIC_REPRESENTATION_ITEM ( )  RATIONAL_B_SPLINE_CURVE ( ( 1.000000000000000222, 0.9510565162951533091, 1.000000000000000000, 0.9510565162951535312, 1.000000000000000000, 0.9510565162951535312, 1.000000000000000000, 0.9510565162951535312, 1.000000000000000000, 0.9510565162951535312, 1.000000000000000000 ) ) 
 REPRESENTATION_ITEM ( '' )  );
#11716 = EDGE_CURVE ( 'NONE', #12336, #10579, #8371, .T. ) ;
#11717 = ORIENTED_EDGE ( 'NONE', *, *, #3248, .F. ) ;
#11718 = ORIENTED_EDGE ( 'NONE', *, *, #12103, .F. ) ;
#11719 = LINE ( 'NONE', #10961, #1162 ) ;
#11720 = ADVANCED_FACE ( 'NONE', ( #6341 ), #3721, .F. ) ;
#11721 = COLOUR_RGB ( '',0.7921568627450980005, 0.8196078431372548767, 0.9333333333333333481 ) ;
#11722 = CARTESIAN_POINT ( 'NONE',  ( 49.99999999999998579, 18.00000000000000355, 169.9999999999999716 ) ) ;
#11723 = CARTESIAN_POINT ( 'NONE',  ( 9.620555948181120698, 22.73892591121550666, 97.77955592743285251 ) ) ;
#11724 = LINE ( 'NONE', #1137, #10503 ) ;
#11725 = CARTESIAN_POINT ( 'NONE',  ( -2.000000000000015543, 20.00000000000000355, 83.29316153445364534 ) ) ;
#11726 = CARTESIAN_POINT ( 'NONE',  ( 4.991728713179328203, 49.66892950866279932, -20.39811079091650114 ) ) ;
#11727 = EDGE_CURVE ( 'NONE', #3312, #5544, #453, .T. ) ;
#11728 = CARTESIAN_POINT ( 'NONE',  ( 27.49999999999999645, 20.00000000000000355, 189.9999999999999716 ) ) ;
#11729 = VECTOR ( 'NONE', #2451, 1000.000000000000000 ) ;
#11730 = CARTESIAN_POINT ( 'NONE',  ( 41.57500000054623257, 24.28113015263587116, 96.68563167572563088 ) ) ;
#11731 = DIRECTION ( 'NONE',  ( -0.000000000000000000, -0.000000000000000000, 1.000000000000000000 ) ) ;
#11732 = EDGE_LOOP ( 'NONE', ( #7650, #6916, #7438 ) ) ;
#11733 = CARTESIAN_POINT ( 'NONE',  ( 7.942143053965557975, 26.11098614794844863, -23.70800582113895061 ) ) ;
#11734 = EDGE_CURVE ( 'NONE', #11952, #11614, #11159, .T. ) ;
#11735 = COLOUR_RGB ( '',0.7921568627450980005, 0.8196078431372548767, 0.9333333333333333481 ) ;
#11736 = CARTESIAN_POINT ( 'NONE',  ( 21.07500000054622191, 24.28113015263587471, 84.90069139318163138 ) ) ;
#11737 = DIRECTION ( 'NONE',  ( -1.000000000000000000, -0.000000000000000000, -0.000000000000000000 ) ) ;
#11738 = CARTESIAN_POINT ( 'NONE',  ( 30.17500000054623044, 13.07298590277314254, 93.04388485072563242 ) ) ;
#11739 = CIRCLE ( 'NONE', #7892, 9.000000000000000000 ) ;
#11740 = CARTESIAN_POINT ( 'NONE',  ( 5.029111531688879921, 11.35041964440615914, -24.49069713376460555 ) ) ;
#11741 = CARTESIAN_POINT ( 'NONE',  ( 24.59999999999998721, 12.86707612778636012, 88.47553407664152303 ) ) ;
#11742 = CARTESIAN_POINT ( 'NONE',  ( 35.27500000054622831, 27.65831843345427998, 90.79316153445363113 ) ) ;
#11743 = ORIENTED_EDGE ( 'NONE', *, *, #9632, .T. ) ;
#11744 = FACE_OUTER_BOUND ( 'NONE', #10314, .T. ) ;
#11745 = ORIENTED_EDGE ( 'NONE', *, *, #12357, .T. ) ;
#11746 = LINE ( 'NONE', #6982, #10551 ) ;
#11747 = ORIENTED_EDGE ( 'NONE', *, *, #396, .F. ) ;
#11748 = DIRECTION ( 'NONE',  ( 0.7071067811865524577, 8.659560562354993255E-17, -0.7071067811865426878 ) ) ;
#11749 = CARTESIAN_POINT ( 'NONE',  ( 5.015793544112643332, 11.34265857438676939, -27.54864687089846598 ) ) ;
#11750 = CARTESIAN_POINT ( 'NONE',  ( 40.47500000054622404, 13.07298590277314432, 88.54243821818161564 ) ) ;
#11751 = DIRECTION ( 'NONE',  ( 0.000000000000000000, 0.000000000000000000, -1.000000000000000000 ) ) ;
#11752 = CARTESIAN_POINT ( 'NONE',  ( 39.87500000054622262, 20.00000000000000355, 98.07665518445361386 ) ) ;
#11753 = CARTESIAN_POINT ( 'NONE',  ( 45.59999999999998721, 27.13292387221364876, 93.11078899226573924 ) ) ;
#11754 = CIRCLE ( 'NONE', #5881, 6.000000000000000000 ) ;
#11755 = CARTESIAN_POINT ( 'NONE',  ( -10.00000000000000355, 20.00000000000000355, 22.91287847477919826 ) ) ;
#11756 = DIRECTION ( 'NONE',  ( 0.000000000000000000, 0.000000000000000000, -1.000000000000000000 ) ) ;
#11757 = ORIENTED_EDGE ( 'NONE', *, *, #2174, .F. ) ;
#11758 = CARTESIAN_POINT ( 'NONE',  ( 34.05000000109246372, 12.86707612778636012, 93.11078899226572503 ) ) ;
#11759 = DIRECTION ( 'NONE',  ( -0.000000000000000000, -1.000000000000000000, -0.000000000000000000 ) ) ;
#11760 = ORIENTED_EDGE ( 'NONE', *, *, #5503, .F. ) ;
#11761 = ORIENTED_EDGE ( 'NONE', *, *, #12344, .F. ) ;
#11762 = AXIS2_PLACEMENT_3D ( 'NONE', #10578, #5895, #1076 ) ;
#11763 = CARTESIAN_POINT ( 'NONE',  ( 5.018193169041119006, 11.34410162984384840, 27.54819609062873198 ) ) ;
#11764 = CARTESIAN_POINT ( 'NONE',  ( 5.000000000000000000, 0.000000000000000000, 0.000000000000000000 ) ) ;
#11765 = EDGE_CURVE ( 'NONE', #7786, #9549, #1519, .T. ) ;
#11766 = CARTESIAN_POINT ( 'NONE',  ( -2.000000000000015543, 20.00000000000000355, 83.29316153445364534 ) ) ;
#11767 = CARTESIAN_POINT ( 'NONE',  ( 29.87500000054622618, 17.63344945572769973, 98.07665518445361386 ) ) ;
#11768 = CARTESIAN_POINT ( 'NONE',  ( 33.07500000054622546, 24.28113015263587471, 84.90069139318163138 ) ) ;
#11769 = CARTESIAN_POINT ( 'NONE',  ( -31.74999999999995737, 0.000000000000000000, 8.000000000000000000 ) ) ;
#11770 = CARTESIAN_POINT ( 'NONE',  ( 31.00470515163596730, 27.49999999999999645, 148.5047051516359318 ) ) ;
#11771 = EDGE_LOOP ( 'NONE', ( #7597, #882, #4075, #2077, #11954, #10502 ) ) ;
#11772 = AXIS2_PLACEMENT_3D ( 'NONE', #2614, #11370, #8454 ) ;
#11773 = CARTESIAN_POINT ( 'NONE',  ( 48.37500000054621552, 12.34168156654572357, 90.79316153445363113 ) ) ;
#11774 = CARTESIAN_POINT ( 'NONE',  ( 47.35000000109245377, 26.37988106264029398, 95.42841645007781892 ) ) ;
#11775 = ORIENTED_EDGE ( 'NONE', *, *, #11212, .F. ) ;
#11776 = CARTESIAN_POINT ( 'NONE',  ( 34.99999999999999289, 15.60660171779822569, 137.5000000000000000 ) ) ;
#11777 = VERTEX_POINT ( 'NONE', #1464 ) ;
#11778 = FACE_OUTER_BOUND ( 'NONE', #3908, .T. ) ;
#11779 = DIRECTION ( 'NONE',  ( 0.000000000000000000, -0.5000000000000012212, -0.8660254037844380415 ) ) ;
#11780 = CARTESIAN_POINT ( 'NONE',  ( -31.74999999999995737, 0.000000000000000000, 0.000000000000000000 ) ) ;
#11781 = CYLINDRICAL_SURFACE ( 'NONE', #4197, 25.00000000000000000 ) ;
#11782 = EDGE_CURVE ( 'NONE', #1317, #9736, #3039, .T. ) ;
#11783 = CARTESIAN_POINT ( 'NONE',  ( 8.867874694687726489, 24.64263244605503900, 96.70324107235252598 ) ) ;
#11784 = DIRECTION ( 'NONE',  ( 1.000000000000000000, -0.000000000000000000, -0.000000000000000000 ) ) ;
#11785 = CARTESIAN_POINT ( 'NONE',  ( -50.00000000000001421, 18.00000000000000355, 188.4007504869563263 ) ) ;
#11786 = CARTESIAN_POINT ( 'NONE',  ( 4.999999999999999112, 22.00000000000000000, 218.7511230907454944 ) ) ;
#11787 = CARTESIAN_POINT ( 'NONE',  ( 10.40000000000000036, 0.000000000000000000, 0.000000000000000000 ) ) ;
#11788 = CARTESIAN_POINT ( 'NONE',  ( 44.27500000054622120, 12.34168156654572535, 90.79316153445363113 ) ) ;
#11789 = CARTESIAN_POINT ( 'NONE',  ( 3.241086154805254083, 10.53405487867120982, 24.79105057270042067 ) ) ;
#11790 = VERTEX_POINT ( 'NONE', #7228 ) ;
#11791 = CARTESIAN_POINT ( 'NONE',  ( -1.643232170762119360, 10.13039557248869471, -27.95362914149064437 ) ) ;
#11792 = APPLICATION_PROTOCOL_DEFINITION ( 'draft international standard', 'automotive_design', 1998, #9995 ) ;
#11793 = DIRECTION ( 'NONE',  ( 0.000000000000000000, -0.5000000000000011102, -0.8660254037844379305 ) ) ;
#11794 = FACE_OUTER_BOUND ( 'NONE', #138, .T. ) ;
#11795 = CARTESIAN_POINT ( 'NONE',  ( 35.37500000054622973, 26.92701409722686634, 93.04388485072563242 ) ) ;
#11796 = CARTESIAN_POINT ( 'NONE',  ( 23.77500000054622475, 22.36655054427230027, 98.07665518445361386 ) ) ;
#11797 = CARTESIAN_POINT ( 'NONE',  ( 24.39999999999998792, 12.86707612778636012, 93.11078899226572503 ) ) ;
#11798 = SURFACE_STYLE_USAGE ( .BOTH. , #7935 ) ;
#11799 = CARTESIAN_POINT ( 'NONE',  ( 25.27500000054622475, 27.65831843345427998, 90.79316153445363113 ) ) ;
#11800 = ORIENTED_EDGE ( 'NONE', *, *, #3016, .F. ) ;
#11801 = ADVANCED_FACE ( 'NONE', ( #2530 ), #9410, .F. ) ;
#11802 = FACE_OUTER_BOUND ( 'NONE', #10284, .T. ) ;
#11803 = DIRECTION ( 'NONE',  ( 1.000000000000000000, 0.000000000000000000, 0.000000000000000000 ) ) ;
#11804 = ORIENTED_EDGE ( 'NONE', *, *, #12125, .T. ) ;
#11805 = CARTESIAN_POINT ( 'NONE',  ( 3.975249800407504974, 53.05026070773460134, 27.71698190627791192 ) ) ;
#11806 = ORIENTED_EDGE ( 'NONE', *, *, #8117, .F. ) ;
#11807 =( NAMED_UNIT ( * ) SI_UNIT ( $, .STERADIAN. ) SOLID_ANGLE_UNIT ( ) );
#11808 = CARTESIAN_POINT ( 'NONE',  ( -2.507735966467860678, 54.33796433351858468, -24.87540749666489148 ) ) ;
#11809 = AXIS2_PLACEMENT_3D ( 'NONE', #4069, #7947, #274 ) ;
#11810 = CARTESIAN_POINT ( 'NONE',  ( -2.000000000000015543, 20.00000000000000355, 90.79316153445363113 ) ) ;
#11811 = EDGE_CURVE ( 'NONE', #2736, #11698, #3264, .T. ) ;
#11812 = CARTESIAN_POINT ( 'NONE',  ( 36.87500000054622262, 20.00000000000000355, 83.50966788445364841 ) ) ;
#11813 = CARTESIAN_POINT ( 'NONE',  ( 0.000000000000000000, 92.00000000000000000, 0.000000000000000000 ) ) ;
#11814 = CARTESIAN_POINT ( 'NONE',  ( 26.59999999999998721, 12.86707612778636012, 88.47553407664152303 ) ) ;
#11815 = CARTESIAN_POINT ( 'NONE',  ( 42.59999999999998721, 12.86707612778636012, 88.47553407664152303 ) ) ;
#11816 = CARTESIAN_POINT ( 'NONE',  ( 39.29999999999999005, 26.37988106264029398, 86.15790661882942914 ) ) ;
#11817 = CARTESIAN_POINT ( 'NONE',  ( 6.000000000000000000, -5.839897972853060892, 7.806255641895631925E-15 ) ) ;
#11818 = VERTEX_POINT ( 'NONE', #10575 ) ;
#11819 = VECTOR ( 'NONE', #6838, 1000.000000000000000 ) ;
#11820 = CARTESIAN_POINT ( 'NONE',  ( 31.85000000109246443, 15.59161060780645691, 96.86078899226572503 ) ) ;
#11821 = CARTESIAN_POINT ( 'NONE',  ( 3.764997658848628692, 46.69378447153945189, -24.71596740620162436 ) ) ;
#11822 = VERTEX_POINT ( 'NONE', #5768 ) ;
#11823 = VERTEX_POINT ( 'NONE', #54 ) ;
#11824 = DIRECTION ( 'NONE',  ( 0.000000000000000000, 0.000000000000000000, 1.000000000000000000 ) ) ;
#11825 = CARTESIAN_POINT ( 'NONE',  ( -5.000000000000000000, 50.00000000000000000, -24.49489742783178059 ) ) ;
#11826 = CARTESIAN_POINT ( 'NONE',  ( 121.9999999999999858, 0.000000000000000000, 0.000000000000000000 ) ) ;
#11827 = AXIS2_PLACEMENT_3D ( 'NONE', #9183, #4291, #5504 ) ;
#11828 = UNCERTAINTY_MEASURE_WITH_UNIT (LENGTH_MEASURE( 1.000000000000000082E-05 ), #4691, 'distance_accuracy_value', 'NONE');
#11829 = CARTESIAN_POINT ( 'NONE',  ( 31.27500000054622831, 27.65831843345427998, 90.79316153445363113 ) ) ;
#11830 = CARTESIAN_POINT ( 'NONE',  ( 28.97500000054622404, 22.36655054427230382, 83.50966788445364841 ) ) ;
#11831 = AXIS2_PLACEMENT_3D ( 'NONE', #1764, #1707, #5713 ) ;
#11832 = CARTESIAN_POINT ( 'NONE',  ( -4.744286179476278953, 51.61208845373312926, 27.59543232531387247 ) ) ;
#11833 = CARTESIAN_POINT ( 'NONE',  ( -8.479561508268508518, 25.31046866060374967, 19.21289678253943478 ) ) ;
#11834 = DIRECTION ( 'NONE',  ( -0.000000000000000000, -0.000000000000000000, 1.000000000000000000 ) ) ;
#11835 = ORIENTED_EDGE ( 'NONE', *, *, #3098, .T. ) ;
#11836 = CARTESIAN_POINT ( 'NONE',  ( 48.17500000054622689, 13.80429023900056507, 95.29460816699764791 ) ) ;
#11837 = CARTESIAN_POINT ( 'NONE',  ( 49.25000000109246656, 27.13292387221364876, 93.11078899226573924 ) ) ;
#11838 = DIRECTION ( 'NONE',  ( 1.000000000000000000, -0.000000000000000000, -0.000000000000000000 ) ) ;
#11839 = ORIENTED_EDGE ( 'NONE', *, *, #9611, .F. ) ;
#11840 = ADVANCED_FACE ( 'NONE', ( #6706 ), #2914, .F. ) ;
#11841 = CARTESIAN_POINT ( 'NONE',  ( 6.000000000000000000, -2.919948986426523341, 5.057500000000002771 ) ) ;
#11842 = ORIENTED_EDGE ( 'NONE', *, *, #2062, .T. ) ;
#11843 = AXIS2_PLACEMENT_3D ( 'NONE', #12332, #12394, #783 ) ;
#11844 = CARTESIAN_POINT ( 'NONE',  ( -2.000000000000015543, 20.00000000000000355, 90.79316153445363113 ) ) ;
#11845 = CARTESIAN_POINT ( 'NONE',  ( -7.295229519525479489, 13.15279342069419499, -23.91310413417861369 ) ) ;
#11846 = ADVANCED_FACE ( 'NONE', ( #1821 ), #11534, .F. ) ;
#11847 = FACE_OUTER_BOUND ( 'NONE', #1839, .T. ) ;
#11848 = LINE ( 'NONE', #9822, #3786 ) ;
#11849 = CARTESIAN_POINT ( 'NONE',  ( 7.063104035062243824, 27.07982170659911958, 93.28061500048886501 ) ) ;
#11850 = CARTESIAN_POINT ( 'NONE',  ( 90.00000000000000000, 0.000000000000000000, 4.171999999999999709 ) ) ;
#11851 = CIRCLE ( 'NONE', #9008, 9.000000000000000000 ) ;
#11852 = DIRECTION ( 'NONE',  ( -1.000000000000000000, -0.000000000000000000, -0.000000000000000000 ) ) ;
#11853 = LINE ( 'NONE', #1203, #5747 ) ;
#11854 = CARTESIAN_POINT ( 'NONE',  ( 121.9999999999999858, 0.000000000000000000, 0.000000000000000000 ) ) ;
#11855 = CARTESIAN_POINT ( 'NONE',  ( 44.77500000054623541, 20.00000000000000355, 83.50966788445364841 ) ) ;
#11856 = CARTESIAN_POINT ( 'NONE',  ( 2.217259272193051967, 45.50669502826730195, 20.88480240601442262 ) ) ;
#11857 = ORIENTED_EDGE ( 'NONE', *, *, #10317, .T. ) ;
#11858 = CARTESIAN_POINT ( 'NONE',  ( 2.571758278209441661E-15, 139.9999999999999716, 21.00000000000000000 ) ) ;
#11859 = EDGE_CURVE ( 'NONE', #9971, #7786, #5707, .T. ) ;
#11860 = ITEM_DEFINED_TRANSFORMATION ( 'NONE', 'NONE', #11018,  #9021 ) ;
#11861 = CIRCLE ( 'NONE', #4555, 7.500000000000007105 ) ;
#11862 = CARTESIAN_POINT ( 'NONE',  ( 21.77500000054622475, 22.36655054427230027, 98.07665518445361386 ) ) ;
#11863 = CARTESIAN_POINT ( 'NONE',  ( 45.07500000054622546, 24.28113015263587471, 84.90069139318163138 ) ) ;
#11864 = ADVANCED_FACE ( 'NONE', ( #11597 ), #7606, .F. ) ;
#11865 = CARTESIAN_POINT ( 'NONE',  ( 36.17500000054622689, 13.07298590277314254, 93.04388485072563242 ) ) ;
#11866 = CARTESIAN_POINT ( 'NONE',  ( 24.47500000054622404, 13.07298590277314432, 88.54243821818161564 ) ) ;
#11867 = CARTESIAN_POINT ( 'NONE',  ( 26.29999999999998295, 13.62011893735971135, 95.42841645007781892 ) ) ;
#11868 = TOROIDAL_SURFACE ( 'NONE', #8024, 8.400000000000000355, 0.5999999999999999778 ) ;
#11869 = B_SPLINE_CURVE_WITH_KNOTS ( 'NONE', 3,
 ( #10057, #1367, #5234, #9105, #8151, #7187, #11065, #6427, #5670, #9597, #2746, #7441, #7632, #6604, #9539, #8458, #839, #12511, #4586, #9417 ),
 .UNSPECIFIED., .F., .F.,
 ( 4, 2, 2, 2, 2, 2, 2, 2, 2, 4 ),
 ( 0.007833776039060080451, 0.008812518928429134007, 0.009791261817798185829, 0.01028063326248271347, 0.01077000470716724112, 0.01174874759653627559, 0.01272749048590531007, 0.01370623337527434801, 0.01468497626464338249, 0.01566371915401241696 ),
 .UNSPECIFIED. ) ;
#11870 = CARTESIAN_POINT ( 'NONE',  ( 49.39999999999998437, 27.13292387221364876, 88.47553407664153724 ) ) ;
#11871 = CARTESIAN_POINT ( 'NONE',  ( 27.97500000054623115, 15.71886984736413417, 96.68563167572563088 ) ) ;
#11872 = ORIENTED_EDGE ( 'NONE', *, *, #94, .T. ) ;
#11873 = CARTESIAN_POINT ( 'NONE',  ( 32.75000000109245946, 22.43689772174679575, 83.29316153445363113 ) ) ;
#11874 = EDGE_LOOP ( 'NONE', ( #5169, #7296, #4834, #10155 ) ) ;
#11875 = ORIENTED_EDGE ( 'NONE', *, *, #12350, .T. ) ;
#11876 = CARTESIAN_POINT ( 'NONE',  ( -20.27158385259951956, 22.00000000000000000, 152.2284161474004520 ) ) ;
#11877 = VERTEX_POINT ( 'NONE', #9636 ) ;
#11878 =( LENGTH_UNIT ( ) NAMED_UNIT ( * ) SI_UNIT ( .MILLI., .METRE. ) );
#11879 = FACE_OUTER_BOUND ( 'NONE', #8758, .T. ) ;
#11880 = CARTESIAN_POINT ( 'NONE',  ( 39.57500000054622546, 26.19570976099943849, 95.29460816699764791 ) ) ;
#11881 = CARTESIAN_POINT ( 'NONE',  ( 39.85000000109246798, 15.59161060780645691, 96.86078899226572503 ) ) ;
#11882 = ADVANCED_FACE ( 'NONE', ( #5828 ), #5640, .T. ) ;
#11883 = CARTESIAN_POINT ( 'NONE',  ( -4.967291850848478241, 49.34246509418954929, -27.55594678612530757 ) ) ;
#11884 = CARTESIAN_POINT ( 'NONE',  ( 38.77500000054622831, 17.63344945572770328, 83.50966788445364841 ) ) ;
#11885 = CARTESIAN_POINT ( 'NONE',  ( 43.19999999999998863, 24.40838939219355197, 84.72553407664153724 ) ) ;
#11886 = CARTESIAN_POINT ( 'NONE',  ( 44.97500000054623115, 24.28113015263587471, 84.90069139318163138 ) ) ;
#11887 = ORIENTED_EDGE ( 'NONE', *, *, #9992, .F. ) ;
#11888 = CARTESIAN_POINT ( 'NONE',  ( 26.75000000109245946, 22.43689772174679575, 83.29316153445363113 ) ) ;
#11889 = LINE ( 'NONE', #3195, #8921 ) ;
#11890 = VECTOR ( 'NONE', #11793, 1000.000000000000114 ) ;
#11891 = EDGE_LOOP ( 'NONE', ( #6616, #1968, #2422, #11456, #6625, #5479 ) ) ;
#11892 = EDGE_CURVE ( 'NONE', #2741, #11966, #813, .T. ) ;
#11893 = CARTESIAN_POINT ( 'NONE',  ( 49.99999999999998579, 0.000000000000000000, 82.99999999999995737 ) ) ;
#11894 = EDGE_LOOP ( 'NONE', ( #2234, #2647 ) ) ;
#11895 = CARTESIAN_POINT ( 'NONE',  ( 7.531311395007206144, 13.38942809998023442, 26.97227661265244336 ) ) ;
#11896 = PLANE ( 'NONE',  #12307 ) ;
#11897 = DIRECTION ( 'NONE',  ( 1.000000000000000000, -0.000000000000000000, -0.000000000000000000 ) ) ;
#11898 = AXIS2_PLACEMENT_3D ( 'NONE', #12480, #8426, #12296 ) ;
#11899 = CARTESIAN_POINT ( 'NONE',  ( 28.27500000054622475, 12.34168156654572535, 90.79316153445363113 ) ) ;
#11900 = CARTESIAN_POINT ( 'NONE',  ( 28.47500000054622404, 13.07298590277314432, 88.54243821818161564 ) ) ;
#11901 = DIRECTION ( 'NONE',  ( -1.000000000000000000, -0.000000000000000000, -0.000000000000000000 ) ) ;
#11902 = CARTESIAN_POINT ( 'NONE',  ( 5.021458388981292487, 28.65403010179421983, 24.49227020900855933 ) ) ;
#11903 = LINE ( 'NONE', #4403, #4015 ) ;
#11904 = ORIENTED_EDGE ( 'NONE', *, *, #4951, .F. ) ;
#11905 = CARTESIAN_POINT ( 'NONE',  ( 5.000000000000000000, 50.00000000000000000, -24.49489742783178414 ) ) ;
#11906 = VERTEX_POINT ( 'NONE', #12365 ) ;
#11907 = DIRECTION ( 'NONE',  ( 1.000000000000000000, 0.000000000000000000, 0.000000000000000000 ) ) ;
#11908 = ORIENTED_EDGE ( 'NONE', *, *, #4882, .T. ) ;
#11909 = AXIS2_PLACEMENT_3D ( 'NONE', #10365, #2759, #6621 ) ;
#11910 = CARTESIAN_POINT ( 'NONE',  ( -5.305379791812843138, 11.51712698327468942, -20.32072021070228018 ) ) ;
#11911 = CARTESIAN_POINT ( 'NONE',  ( 10.40000000000000036, 6.613092715395708453E-16, 5.400000000000001243 ) ) ;
#11912 = DIRECTION ( 'NONE',  ( -1.000000000000000000, -0.000000000000000000, -0.000000000000000000 ) ) ;
#11913 = AXIS2_PLACEMENT_3D ( 'NONE', #79, #5975, #4839 ) ;
#11914 = CARTESIAN_POINT ( 'NONE',  ( 6.731970158774189805, 27.39502174583683569, 89.51723080467371574 ) ) ;
#11915 = CARTESIAN_POINT ( 'NONE',  ( 2.213389590484158731, 45.51360200414269741, -24.90224851187377553 ) ) ;
#11916 = CARTESIAN_POINT ( 'NONE',  ( -3.974640651900942512, 46.94910328357455143, -24.68270373814292640 ) ) ;
#11917 = CARTESIAN_POINT ( 'NONE',  ( -4.999999999999999112, 50.32699065753391920, 20.39607805437114152 ) ) ;
#11918 = CARTESIAN_POINT ( 'NONE',  ( 7.302632803679189877, 26.83934157082542882, -19.69087995796197887 ) ) ;
#11919 = CARTESIAN_POINT ( 'NONE',  ( 43.87500000054622973, 17.63344945572769973, 98.07665518445361386 ) ) ;
#11920 = DIRECTION ( 'NONE',  ( -1.000000000000000000, -0.000000000000000000, -0.000000000000000000 ) ) ;
#11921 = ORIENTED_EDGE ( 'NONE', *, *, #10383, .T. ) ;
#11922 = VECTOR ( 'NONE', #10482, 1000.000000000000000 ) ;
#11923 = CARTESIAN_POINT ( 'NONE',  ( 0.6000000000000033085, 0.000000000000000000, 9.000000000000000000 ) ) ;
#11924 = ADVANCED_FACE ( 'NONE', ( #3667 ), #6770, .T. ) ;
#11925 = CARTESIAN_POINT ( 'NONE',  ( 21.97500000054622049, 17.63344945572769973, 98.07665518445361386 ) ) ;
#11926 = CARTESIAN_POINT ( 'NONE',  ( 42.07500000054622546, 15.71886984736413417, 96.68563167572563088 ) ) ;
#11927 = CARTESIAN_POINT ( 'NONE',  ( 30.87500000054622618, 22.36655054427230382, 83.50966788445364841 ) ) ;
#11928 =( BOUNDED_CURVE ( )  B_SPLINE_CURVE ( 3, ( #994, #9747, #232, #7714 ),
 .UNSPECIFIED., .F., .F. ) 
 B_SPLINE_CURVE_WITH_KNOTS ( ( 4, 4 ),
 ( -8.881784197001252323E-16, 1.570796326794896558 ),
 .UNSPECIFIED. ) 
 CURVE ( )  GEOMETRIC_REPRESENTATION_ITEM ( )  RATIONAL_B_SPLINE_CURVE ( ( 1.000000000000000000, 0.8047378541243648264, 0.8047378541243648264, 1.000000000000000000 ) ) 
 REPRESENTATION_ITEM ( '' )  );
#11929 = AXIS2_PLACEMENT_3D ( 'NONE', #11022, #9252, #7209 ) ;
#11930 = CARTESIAN_POINT ( 'NONE',  ( 0.000000000000000000, 139.9999999999999716, 0.000000000000000000 ) ) ;
#11931 = DIRECTION ( 'NONE',  ( -1.000000000000000000, -0.000000000000000000, -0.000000000000000000 ) ) ;
#11932 = CARTESIAN_POINT ( 'NONE',  ( 49.69999999999998863, 26.37988106264029398, 95.42841645007781892 ) ) ;
#11933 = CARTESIAN_POINT ( 'NONE',  ( 23.77500000054622831, 20.00000000000000355, 98.07665518445361386 ) ) ;
#11934 = ORIENTED_EDGE ( 'NONE', *, *, #10015, .F. ) ;
#11935 = CARTESIAN_POINT ( 'NONE',  ( 23.35000000109246443, 26.37988106264029398, 95.42841645007781892 ) ) ;
#11936 = ORIENTED_EDGE ( 'NONE', *, *, #8133, .F. ) ;
#11937 = ORIENTED_EDGE ( 'NONE', *, *, #5045, .T. ) ;
#11938 = DIRECTION ( 'NONE',  ( 0.000000000000000000, 0.000000000000000000, 1.000000000000000000 ) ) ;
#11939 = ORIENTED_EDGE ( 'NONE', *, *, #5368, .T. ) ;
#11940 = DIRECTION ( 'NONE',  ( 0.000000000000000000, 0.000000000000000000, -1.000000000000000000 ) ) ;
#11941 =( REPRESENTATION_RELATIONSHIP ('NONE','NONE', #4262, #10815 ) REPRESENTATION_RELATIONSHIP_WITH_TRANSFORMATION ( #2457 )SHAPE_REPRESENTATION_RELATIONSHIP( ) );
#11942 = CARTESIAN_POINT ( 'NONE',  ( 37.17500000054621978, 26.19570976099943849, 86.29171490190961435 ) ) ;
#11943 = CARTESIAN_POINT ( 'NONE',  ( 92.00000000000000000, 0.000000000000000000, 5.035999999999999588 ) ) ;
#11944 = CARTESIAN_POINT ( 'NONE',  ( 20.65000000109246514, 20.00000000000000355, 83.29316153445364534 ) ) ;
#11945 = CARTESIAN_POINT ( 'NONE',  ( 37.87500000054622262, 20.00000000000000355, 98.07665518445361386 ) ) ;
#11946 = CARTESIAN_POINT ( 'NONE',  ( 39.19999999999998153, 24.40838939219355197, 84.72553407664153724 ) ) ;
#11947 = ADVANCED_FACE ( 'NONE', ( #9573, #8740 ), #3917, .T. ) ;
#11948 = CARTESIAN_POINT ( 'NONE',  ( 45.17500000054622689, 26.92701409722686634, 88.54243821818162985 ) ) ;
#11949 = EDGE_LOOP ( 'NONE', ( #11413, #4387, #11573, #2693, #7499, #8753 ) ) ;
#11950 = CARTESIAN_POINT ( 'NONE',  ( 25.95000000109246585, 13.62011893735971135, 95.42841645007781892 ) ) ;
#11951 = CARTESIAN_POINT ( 'NONE',  ( -8.967015720386880773, 15.56160195868188545, 23.33709189419391805 ) ) ;
#11952 = VERTEX_POINT ( 'NONE', #2971 ) ;
#11953 = CARTESIAN_POINT ( 'NONE',  ( -9.467453437281745821, 23.23658378093145771, -26.35104892248523356 ) ) ;
#11954 = ORIENTED_EDGE ( 'NONE', *, *, #5634, .F. ) ;
#11955 = FACE_OUTER_BOUND ( 'NONE', #3574, .T. ) ;
#11956 = CARTESIAN_POINT ( 'NONE',  ( 40.95000000109246940, 26.37988106264029398, 86.15790661882942914 ) ) ;
#11957 = CARTESIAN_POINT ( 'NONE',  ( 25.29999999999998295, 26.37988106264029398, 86.15790661882942914 ) ) ;
#11958 = CARTESIAN_POINT ( 'NONE',  ( 31.47500000054623115, 26.19570976099943493, 95.29460816699764791 ) ) ;
#11959 = CARTESIAN_POINT ( 'NONE',  ( 32.77500000054622831, 17.63344945572770328, 83.50966788445364841 ) ) ;
#11960 = EDGE_CURVE ( 'NONE', #2177, #4738, #1702, .T. ) ;
#11961 = PLANE ( 'NONE',  #8595 ) ;
#11962 = LINE ( 'NONE', #11007, #2790 ) ;
#11963 = EDGE_LOOP ( 'NONE', ( #11136, #1647, #1844, #10534, #1773 ) ) ;
#11964 = CARTESIAN_POINT ( 'NONE',  ( 42.95000000109246940, 26.37988106264029398, 86.15790661882942914 ) ) ;
#11965 =( NAMED_UNIT ( * ) PLANE_ANGLE_UNIT ( ) SI_UNIT ( $, .RADIAN. ) );
#11966 = VERTEX_POINT ( 'NONE', #3223 ) ;
#11967 = DIRECTION ( 'NONE',  ( -1.000000000000000000, -0.000000000000000000, -0.000000000000000000 ) ) ;
#11968 = AXIS2_PLACEMENT_3D ( 'NONE', #6788, #1090, #2092 ) ;
#11969 = EDGE_CURVE ( 'NONE', #4011, #5701, #10506, .T. ) ;
#11970 = VERTEX_POINT ( 'NONE', #5951 ) ;
#11971 = DIRECTION ( 'NONE',  ( 0.000000000000000000, 0.000000000000000000, 1.000000000000000000 ) ) ;
#11972 = CARTESIAN_POINT ( 'NONE',  ( 9.868114579493717287, 18.34823788458374594, -22.97009550651098309 ) ) ;
#11973 = CARTESIAN_POINT ( 'NONE',  ( 0.6000000000000033085, 1.028703311283776586E-15, -8.400000000000000355 ) ) ;
#11974 = EDGE_CURVE ( 'NONE', #8129, #2202, #5767, .T. ) ;
#11975 = AXIS2_PLACEMENT_3D ( 'NONE', #8954, #12061, #6344 ) ;
#11976 = CARTESIAN_POINT ( 'NONE',  ( 3.764018802651051487, 53.30721710162806204, 24.71610890024348350 ) ) ;
#11977 = PRODUCT_DEFINITION_SHAPE ( 'NONE', 'NONE',  #12544 ) ;
#11978 = CARTESIAN_POINT ( 'NONE',  ( 37.75000000109245946, 17.56310227825323977, 98.29316153445364534 ) ) ;
#11979 = CARTESIAN_POINT ( 'NONE',  ( -50.00000000000001421, 20.00000000000000000, 145.0000000000000000 ) ) ;
#11980 = CARTESIAN_POINT ( 'NONE',  ( -5.000000000000000888, 49.67303160952345564, -24.49489742783178059 ) ) ;
#11981 = CARTESIAN_POINT ( 'NONE',  ( 5.000000000000000000, -3.513898075855362180, -2.028749999999995168 ) ) ;
#11982 = CARTESIAN_POINT ( 'NONE',  ( -5.000000000000000000, 50.00000000000000000, 27.54995462791182348 ) ) ;
#11983 = CARTESIAN_POINT ( 'NONE',  ( -2.217037138455994150, 45.50647851044359982, -24.90334479454202921 ) ) ;
#11984 = ORIENTED_EDGE ( 'NONE', *, *, #7772, .F. ) ;
#11985 = CIRCLE ( 'NONE', #9145, 26.49999999999999645 ) ;
#11986 = CARTESIAN_POINT ( 'NONE',  ( -0.3301821175306443035, 55.00000000000001421, 25.00000000000000000 ) ) ;
#11987 = CARTESIAN_POINT ( 'NONE',  ( 3.061565168526138680E-15, 55.00000000000000000, 25.00000000000000000 ) ) ;
#11988 = CARTESIAN_POINT ( 'NONE',  ( 45.47500000054622404, 26.92701409722686634, 93.04388485072563242 ) ) ;
#11989 = CIRCLE ( 'NONE', #10355, 5.999999999999999112 ) ;
#11990 = CARTESIAN_POINT ( 'NONE',  ( 26.57500000054622902, 15.71886984736413773, 84.90069139318163138 ) ) ;
#11991 = CARTESIAN_POINT ( 'NONE',  ( 9.240229740357481347, 16.15179536300817986, 97.24847665116462281 ) ) ;
#11992 = CARTESIAN_POINT ( 'NONE',  ( 19.99999999999998579, 20.00000000000000355, 98.29316153445363113 ) ) ;
#11993 = CARTESIAN_POINT ( 'NONE',  ( 6.000000000000000000, -2.919948986426523341, 5.057500000000002771 ) ) ;
#11994 = CARTESIAN_POINT ( 'NONE',  ( 25.87500000054622262, 17.63344945572769973, 98.07665518445361386 ) ) ;
#11995 = ORIENTED_EDGE ( 'NONE', *, *, #10099, .T. ) ;
#11996 = FACE_OUTER_BOUND ( 'NONE', #3951, .T. ) ;
#11997 = ORIENTED_EDGE ( 'NONE', *, *, #11727, .F. ) ;
#11998 = ORIENTED_EDGE ( 'NONE', *, *, #10029, .T. ) ;
#11999 = EDGE_CURVE ( 'NONE', #8904, #12216, #4173, .T. ) ;
#12000 = DIRECTION ( 'NONE',  ( -1.000000000000000000, 0.000000000000000000, 0.000000000000000000 ) ) ;
#12001 = ORIENTED_EDGE ( 'NONE', *, *, #561, .T. ) ;
#12002 =( BOUNDED_CURVE ( )  B_SPLINE_CURVE ( 3, ( #4365, #3095, #3163, #7028 ),
 .UNSPECIFIED., .F., .F. ) 
 B_SPLINE_CURVE_WITH_KNOTS ( ( 4, 4 ),
 ( -8.881784197001252323E-16, 1.570796326794896558 ),
 .UNSPECIFIED. ) 
 CURVE ( )  GEOMETRIC_REPRESENTATION_ITEM ( )  RATIONAL_B_SPLINE_CURVE ( ( 1.000000000000000000, 0.8047378541243648264, 0.8047378541243648264, 1.000000000000000000 ) ) 
 REPRESENTATION_ITEM ( '' )  );
#12003 = CARTESIAN_POINT ( 'NONE',  ( 30.87500000054622618, 20.00000000000000355, 83.50966788445364841 ) ) ;
#12004 = CARTESIAN_POINT ( 'NONE',  ( 6.000000000000000000, 2.919948986426538884, 5.057499999999996554 ) ) ;
#12005 = DIRECTION ( 'NONE',  ( 0.000000000000000000, -1.000000000000000000, 0.000000000000000000 ) ) ;
#12006 = CARTESIAN_POINT ( 'NONE',  ( 40.67500000054622689, 15.71886984736413773, 84.90069139318163138 ) ) ;
#12007 = CARTESIAN_POINT ( 'NONE',  ( 35.09999999999998721, 22.43689772174679575, 83.29316153445363113 ) ) ;
#12008 = CARTESIAN_POINT ( 'NONE',  ( 43.17500000054622689, 26.92701409722686634, 88.54243821818162985 ) ) ;
#12009 = ORIENTED_EDGE ( 'NONE', *, *, #7622, .F. ) ;
#12010 = CARTESIAN_POINT ( 'NONE',  ( 22.65000000109246514, 20.00000000000000355, 83.29316153445364534 ) ) ;
#12011 = CARTESIAN_POINT ( 'NONE',  ( -9.983814731900727324, 19.34254964819328038, 22.91996290304706108 ) ) ;
#12012 = ORIENTED_EDGE ( 'NONE', *, *, #4287, .T. ) ;
#12013 = CARTESIAN_POINT ( 'NONE',  ( -10.00000000000000355, 20.65909654603918355, -26.15339366124404563 ) ) ;
#12014 = VERTEX_POINT ( 'NONE', #248 ) ;
#12015 = AXIS2_PLACEMENT_3D ( 'NONE', #12004, #7298, #4321 ) ;
#12016 = LINE ( 'NONE', #7894, #7280 ) ;
#12017 = EDGE_CURVE ( 'NONE', #7940, #2752, #5978, .T. ) ;
#12018 = DIRECTION ( 'NONE',  ( -1.000000000000000000, 0.000000000000000000, 0.000000000000000000 ) ) ;
#12019 = CARTESIAN_POINT ( 'NONE',  ( 25.59999999999998721, 27.13292387221364876, 93.11078899226573924 ) ) ;
#12020 = CARTESIAN_POINT ( 'NONE',  ( 31.97500000054623470, 15.71886984736413417, 96.68563167572563088 ) ) ;
#12021 = CARTESIAN_POINT ( 'NONE',  ( 22.47500000054622404, 13.07298590277314432, 88.54243821818161564 ) ) ;
#12022 = ADVANCED_FACE ( 'NONE', ( #3978 ), #9063, .F. ) ;
#12023 = CIRCLE ( 'NONE', #3916, 4.171999999999999709 ) ;
#12024 = CARTESIAN_POINT ( 'NONE',  ( 49.93750000027311131, 20.00000000000000355, 98.18490835945361539 ) ) ;
#12025 = CARTESIAN_POINT ( 'NONE',  ( -2.000000000000015543, 20.00000000000000355, 83.29316153445364534 ) ) ;
#12026 = ORIENTED_EDGE ( 'NONE', *, *, #11635, .T. ) ;
#12027 = CARTESIAN_POINT ( 'NONE',  ( 44.75000000109245946, 22.43689772174679575, 83.29316153445363113 ) ) ;
#12028 = CARTESIAN_POINT ( 'NONE',  ( 4.999999999999999112, 50.32998418051842293, -24.49489742783177348 ) ) ;
#12029 = ORIENTED_EDGE ( 'NONE', *, *, #1952, .F. ) ;
#12030 = CARTESIAN_POINT ( 'NONE',  ( 11.99999999999999645, 1.102182119232617714E-15, -9.000000000000000000 ) ) ;
#12031 = ORIENTED_EDGE ( 'NONE', *, *, #2235, .T. ) ;
#12032 = CARTESIAN_POINT ( 'NONE',  ( -9.349016511544222752, 16.43577148148449396, -18.80467678224717432 ) ) ;
#12033 = EDGE_CURVE ( 'NONE', #2177, #4576, #2926, .T. ) ;
#12034 = TOROIDAL_SURFACE ( 'NONE', #6551, 17.50000000000000355, 10.00000000000000000 ) ;
#12035 = CARTESIAN_POINT ( 'NONE',  ( -5.025242304149237782, 28.65182443915274746, 24.49149081028624053 ) ) ;
#12036 = AXIS2_PLACEMENT_3D ( 'NONE', #2726, #760, #12372 ) ;
#12037 = LINE ( 'NONE', #3339, #2510 ) ;
#12038 = ADVANCED_FACE ( 'NONE', ( #10827 ), #2452, .T. ) ;
#12039 = CARTESIAN_POINT ( 'NONE',  ( -6.999999999999999112, 77.00000000000000000, 146.8533255156881978 ) ) ;
#12040 = PLANE ( 'NONE',  #11929 ) ;
#12041 = CIRCLE ( 'NONE', #5757, 5.057500000000000107 ) ;
#12042 = CARTESIAN_POINT ( 'NONE',  ( 0.6000000000000033085, 0.000000000000000000, 0.000000000000000000 ) ) ;
#12043 = CARTESIAN_POINT ( 'NONE',  ( -7.944152373534001832, 13.89170734695355058, 26.85206817267833657 ) ) ;
#12044 = CARTESIAN_POINT ( 'NONE',  ( 5.316967106970424517, 28.47548153940854831, -20.31764798226379654 ) ) ;
#12045 = AXIS2_PLACEMENT_3D ( 'NONE', #539, #11130, #5238 ) ;
#12046 = EDGE_CURVE ( 'NONE', #2612, #6710, #11851, .T. ) ;
#12047 = CARTESIAN_POINT ( 'NONE',  ( -5.000000000000000000, 50.00000000000000000, -24.49489742783178059 ) ) ;
#12048 = EDGE_LOOP ( 'NONE', ( #270, #1161, #10602, #789 ) ) ;
#12049 = EDGE_CURVE ( 'NONE', #949, #10115, #8802, .T. ) ;
#12050 = LINE ( 'NONE', #11858, #12324 ) ;
#12051 = CARTESIAN_POINT ( 'NONE',  ( 5.000000000000000000, -2.342598717236911821, -4.057499999999996554 ) ) ;
#12052 = TOROIDAL_SURFACE ( 'NONE', #10612, 6.599999999999998757, 0.5999999999999999778 ) ;
#12053 = CARTESIAN_POINT ( 'NONE',  ( 3.429011037612589670E-15, -4.262400816306111331E-15, 28.00000000000000355 ) ) ;
#12054 = CARTESIAN_POINT ( 'NONE',  ( 45.27500000054622831, 26.92701409722686634, 88.54243821818162985 ) ) ;
#12055 = CARTESIAN_POINT ( 'NONE',  ( 26.87500000054622618, 22.36655054427230382, 83.50966788445364841 ) ) ;
#12056 = DIRECTION ( 'NONE',  ( 0.000000000000000000, 1.000000000000000000, -1.295896757998781374E-15 ) ) ;
#12057 = DIRECTION ( 'NONE',  ( -1.000000000000000000, 0.000000000000000000, 0.000000000000000000 ) ) ;
#12058 = CARTESIAN_POINT ( 'NONE',  ( 35.29999999999998295, 26.37988106264029398, 86.15790661882942914 ) ) ;
#12059 = CARTESIAN_POINT ( 'NONE',  ( -111.8465843842649292, 77.00000000000000000, 101.8533255156881978 ) ) ;
#12060 = EDGE_LOOP ( 'NONE', ( #11320, #6900, #1156, #11638, #3779, #9974 ) ) ;
#12061 = DIRECTION ( 'NONE',  ( 1.000000000000000000, 0.000000000000000000, 0.000000000000000000 ) ) ;
#12062 = ORIENTED_EDGE ( 'NONE', *, *, #7656, .T. ) ;
#12063 = CARTESIAN_POINT ( 'NONE',  ( 5.000000000000000000, 0.000000000000000000, 0.000000000000000000 ) ) ;
#12064 = AXIS2_PLACEMENT_3D ( 'NONE', #2888, #10307, #1624 ) ;
#12065 = VERTEX_POINT ( 'NONE', #3470 ) ;
#12066 =( LENGTH_UNIT ( ) NAMED_UNIT ( * ) SI_UNIT ( .MILLI., .METRE. ) );
#12067 = CARTESIAN_POINT ( 'NONE',  ( 28.97500000054622404, 22.36655054427230382, 83.50966788445364841 ) ) ;
#12068 = CARTESIAN_POINT ( 'NONE',  ( -4.967628512179818046, 50.65508169058694676, -27.55588583811023895 ) ) ;
#12069 = CARTESIAN_POINT ( 'NONE',  ( 46.47500000054623115, 13.80429023900056684, 86.29171490190961435 ) ) ;
#12070 = CARTESIAN_POINT ( 'NONE',  ( 31.17500000054621978, 26.19570976099943493, 86.29171490190961435 ) ) ;
#12071 = CARTESIAN_POINT ( 'NONE',  ( 34.99999999999999289, 20.00000000000000355, 83.29316153445364534 ) ) ;
#12072 = CARTESIAN_POINT ( 'NONE',  ( 43.97500000054623115, 15.71886984736413417, 96.68563167572563088 ) ) ;
#12073 = VERTEX_POINT ( 'NONE', #12166 ) ;
#12074 = CARTESIAN_POINT ( 'NONE',  ( 23.05000000109246372, 27.13292387221364876, 88.47553407664153724 ) ) ;
#12075 = CARTESIAN_POINT ( 'NONE',  ( -7.536850167683876833, 13.39586159374066021, 23.84162237519015548 ) ) ;
#12076 = ORIENTED_EDGE ( 'NONE', *, *, #8202, .T. ) ;
#12077 = DIRECTION ( 'NONE',  ( 1.000000000000000000, -0.000000000000000000, -0.000000000000000000 ) ) ;
#12078 = CIRCLE ( 'NONE', #7405, 0.5999999999999998668 ) ;
#12079 = ORIENTED_EDGE ( 'NONE', *, *, #6207, .T. ) ;
#12080 = CARTESIAN_POINT ( 'NONE',  ( 6.000000000000000000, 2.919948986426526005, -5.057500000000003659 ) ) ;
#12081 = DIRECTION ( 'NONE',  ( 1.000000000000000000, 0.000000000000000000, 0.000000000000000000 ) ) ;
#12082 = CARTESIAN_POINT ( 'NONE',  ( 35.85000000109246798, 15.59161060780645691, 96.86078899226572503 ) ) ;
#12083 = CARTESIAN_POINT ( 'NONE',  ( 0.000000000000000000, 20.00000000000000355, -70.00000000000000000 ) ) ;
#12084 = ADVANCED_FACE ( 'NONE', ( #9189 ), #12052, .F. ) ;
#12085 = CARTESIAN_POINT ( 'NONE',  ( 22.67500000054622333, 17.63344945572770328, 83.50966788445364841 ) ) ;
#12086 = CARTESIAN_POINT ( 'NONE',  ( 25.27500000054622475, 26.92701409722686634, 88.54243821818162985 ) ) ;
#12087 = LINE ( 'NONE', #3206, #3127 ) ;
#12088 = CARTESIAN_POINT ( 'NONE',  ( -1.612909136089518691, 45.25592802960594696, 24.94976847917136453 ) ) ;
#12089 = ORIENTED_EDGE ( 'NONE', *, *, #3433, .F. ) ;
#12090 = CARTESIAN_POINT ( 'NONE',  ( 41.55000000109246372, 22.43689772174679575, 98.29316153445363113 ) ) ;
#12091 = PRESENTATION_STYLE_ASSIGNMENT (( #1314 ) ) ;
#12092 = ORIENTED_EDGE ( 'NONE', *, *, #6966, .T. ) ;
#12093 = CARTESIAN_POINT ( 'NONE',  ( 47.69999999999999574, 26.37988106264029398, 95.42841645007781892 ) ) ;
#12094 = ORIENTED_EDGE ( 'NONE', *, *, #11782, .T. ) ;
#12095 = LINE ( 'NONE', #6440, #4643 ) ;
#12096 = AXIS2_PLACEMENT_3D ( 'NONE', #5633, #2965, #2902 ) ;
#12097 = EDGE_CURVE ( 'NONE', #11275, #12065, #2517, .T. ) ;
#12098 = CARTESIAN_POINT ( 'NONE',  ( 25.65000000109246514, 20.00000000000000355, 98.29316153445363113 ) ) ;
#12099 = CARTESIAN_POINT ( 'NONE',  ( 20.87500000054622973, 22.36655054427230382, 83.50966788445364841 ) ) ;
#12100 = CARTESIAN_POINT ( 'NONE',  ( 5.000000000000000000, -2.342598717236902051, 4.057500000000004547 ) ) ;
#12101 = CARTESIAN_POINT ( 'NONE',  ( 10.00000000000000355, 20.00000000000000355, -28.00000000000000711 ) ) ;
#12102 = EDGE_CURVE ( 'NONE', #8208, #5738, #9124, .T. ) ;
#12103 = EDGE_CURVE ( 'NONE', #7957, #2444, #11574, .T. ) ;
#12104 = CARTESIAN_POINT ( 'NONE',  ( 6.000000000000000000, 5.839897972853065333, -6.938893903907228378E-15 ) ) ;
#12105 = DIRECTION ( 'NONE',  ( 0.000000000000000000, 0.000000000000000000, -1.000000000000000000 ) ) ;
#12106 = AXIS2_PLACEMENT_3D ( 'NONE', #4480, #6607, #9600 ) ;
#12107 = CARTESIAN_POINT ( 'NONE',  ( 3.547335893868845513, 29.35536450536750408, 24.74892486337281738 ) ) ;
#12108 = CARTESIAN_POINT ( 'NONE',  ( -3.306342958134543153, 53.76488593550792672, 24.78149064010515445 ) ) ;
#12109 = ORIENTED_EDGE ( 'NONE', *, *, #985, .F. ) ;
#12110 = ADVANCED_FACE ( 'NONE', ( #8173 ), #1386, .T. ) ;
#12111 = CARTESIAN_POINT ( 'NONE',  ( 12.00000000000000178, 0.000000000000000000, 0.000000000000000000 ) ) ;
#12112 = AXIS2_PLACEMENT_3D ( 'NONE', #8352, #6322, #10072 ) ;
#12113 = DIRECTION ( 'NONE',  ( 0.000000000000000000, 0.000000000000000000, 1.000000000000000000 ) ) ;
#12114 = CARTESIAN_POINT ( 'NONE',  ( 44.67500000054621978, 15.71886984736413773, 84.90069139318163138 ) ) ;
#12115 = CARTESIAN_POINT ( 'NONE',  ( 23.67500000054622333, 22.36655054427230027, 98.07665518445361386 ) ) ;
#12116 = EDGE_CURVE ( 'NONE', #2612, #7043, #11032, .T. ) ;
#12117 = CARTESIAN_POINT ( 'NONE',  ( 8.653999659896598473, 14.97853430653165319, -23.45497003317995421 ) ) ;
#12118 = DIRECTION ( 'NONE',  ( 1.000000000000000000, -0.000000000000000000, -0.000000000000000000 ) ) ;
#12119 = CARTESIAN_POINT ( 'NONE',  ( 33.69999999999998153, 26.37988106264029398, 95.42841645007781892 ) ) ;
#12120 = FACE_OUTER_BOUND ( 'NONE', #5724, .T. ) ;
#12121 = ORIENTED_EDGE ( 'NONE', *, *, #1399, .T. ) ;
#12122 = CARTESIAN_POINT ( 'NONE',  ( 23.55000000109246017, 22.43689772174679575, 98.29316153445363113 ) ) ;
#12123 = DIRECTION ( 'NONE',  ( 0.4999999999999892308, 0.000000000000000000, 0.8660254037844448138 ) ) ;
#12124 = ORIENTED_EDGE ( 'NONE', *, *, #3025, .T. ) ;
#12125 = EDGE_CURVE ( 'NONE', #8255, #7452, #10371, .T. ) ;
#12126 = VECTOR ( 'NONE', #2016, 1000.000000000000000 ) ;
#12127 = CARTESIAN_POINT ( 'NONE',  ( 30.97500000054622404, 22.36655054427230382, 83.50966788445364841 ) ) ;
#12128 = DIRECTION ( 'NONE',  ( 0.000000000000000000, 0.000000000000000000, -1.000000000000000000 ) ) ;
#12129 = CARTESIAN_POINT ( 'NONE',  ( 44.17500000054622689, 13.07298590277314254, 93.04388485072563242 ) ) ;
#12130 = CARTESIAN_POINT ( 'NONE',  ( 32.37500000054621552, 12.34168156654572535, 90.79316153445363113 ) ) ;
#12131 = CARTESIAN_POINT ( 'NONE',  ( 35.59999999999998721, 27.13292387221364876, 93.11078899226573924 ) ) ;
#12132 = CARTESIAN_POINT ( 'NONE',  ( -7.926973682980901437, 26.10475523195332315, 19.44767585397084986 ) ) ;
#12133 = CARTESIAN_POINT ( 'NONE',  ( 48.47500000054623115, 13.80429023900056684, 86.29171490190961435 ) ) ;
#12134 = EDGE_LOOP ( 'NONE', ( #6743, #11857, #12137, #1053 ) ) ;
#12135 = CARTESIAN_POINT ( 'NONE',  ( 23.65000000109246514, 20.00000000000000355, 98.29316153445363113 ) ) ;
#12136 = CARTESIAN_POINT ( 'NONE',  ( -2.505953076466797658, 45.67021871533034982, 24.87450930309000441 ) ) ;
#12137 = ORIENTED_EDGE ( 'NONE', *, *, #6410, .T. ) ;
#12138 = CIRCLE ( 'NONE', #1989, 0.5999999999999998668 ) ;
#12139 = FACE_OUTER_BOUND ( 'NONE', #7942, .T. ) ;
#12140 = ORIENTED_EDGE ( 'NONE', *, *, #8777, .T. ) ;
#12141 = CARTESIAN_POINT ( 'NONE',  ( 19.87500000054622262, 20.00000000000000355, 98.07665518445361386 ) ) ;
#12142 = CARTESIAN_POINT ( 'NONE',  ( 10.00000000000000000, 8.000000000000000000, 0.000000000000000000 ) ) ;
#12143 = CARTESIAN_POINT ( 'NONE',  ( 35.65000000109246514, 20.00000000000000355, 98.29316153445363113 ) ) ;
#12144 = DIRECTION ( 'NONE',  ( 1.000000000000000000, 0.000000000000000000, 0.000000000000000000 ) ) ;
#12145 = AXIS2_PLACEMENT_3D ( 'NONE', #9331, #1643, #7417 ) ;
#12146 = CARTESIAN_POINT ( 'NONE',  ( 26.77500000054622831, 20.00000000000000355, 83.50966788445364841 ) ) ;
#12147 = CARTESIAN_POINT ( 'NONE',  ( 22.37500000054622262, 12.34168156654572535, 90.79316153445363113 ) ) ;
#12148 = CARTESIAN_POINT ( 'NONE',  ( 3.235823500505065287, 29.46772395162260594, 27.81419857650566385 ) ) ;
#12149 = AXIS2_PLACEMENT_3D ( 'NONE', #10659, #6544, #4706 ) ;
#12150 = CARTESIAN_POINT ( 'NONE',  ( 22.55000000109246017, 17.56310227825320425, 83.29316153445363113 ) ) ;
#12151 = VERTEX_POINT ( 'NONE', #4606 ) ;
#12152 = CARTESIAN_POINT ( 'NONE',  ( 41.25000000109246656, 27.13292387221364876, 93.11078899226573924 ) ) ;
#12153 = LINE ( 'NONE', #10003, #12327 ) ;
#12154 = ORIENTED_EDGE ( 'NONE', *, *, #3973, .T. ) ;
#12155 = CARTESIAN_POINT ( 'NONE',  ( 30.45000000109246585, 15.59161060780646046, 84.72553407664153724 ) ) ;
#12156 = ORIENTED_EDGE ( 'NONE', *, *, #5454, .F. ) ;
#12157 = EDGE_CURVE ( 'NONE', #10127, #949, #931, .T. ) ;
#12158 = CARTESIAN_POINT ( 'NONE',  ( -7.295229519525479489, 13.15279342069419499, -23.91310413417861369 ) ) ;
#12159 = DIRECTION ( 'NONE',  ( 0.000000000000000000, 0.000000000000000000, 1.000000000000000000 ) ) ;
#12160 = DIRECTION ( 'NONE',  ( 0.000000000000000000, 0.000000000000000000, 1.000000000000000000 ) ) ;
#12161 = B_SPLINE_CURVE_WITH_KNOTS ( 'NONE', 3,
 ( #732, #12343, #3643, #11388, #8973, #6812, #32, #8025, #9803, #5046, #4083, #8778, #2117, #4917, #4150, #3071, #97, #1986 ),
 .UNSPECIFIED., .F., .F.,
 ( 4, 2, 2, 2, 2, 2, 2, 2, 4 ),
 ( 5.188175463412582976E-20, 0.0009797360301013575360, 0.001959472060202715072, 0.002939208090304072825, 0.003918944120405430144, 0.004898680150506787463, 0.005878416180608145650, 0.006858152210709502969, 0.007837888240810860288 ),
 .UNSPECIFIED. ) ;
#12162 = SURFACE_STYLE_USAGE ( .BOTH. , #4294 ) ;
#12163 = PLANE ( 'NONE',  #709 ) ;
#12164 = CARTESIAN_POINT ( 'NONE',  ( 49.99999999999998579, 20.00000000000000000, 137.5000000000000000 ) ) ;
#12165 = AXIS2_PLACEMENT_3D ( 'NONE', #3743, #8390, #6538 ) ;
#12166 = CARTESIAN_POINT ( 'NONE',  ( 32.00000000000000000, 0.000000000000000000, 5.035999999999999588 ) ) ;
#12167 = DIRECTION ( 'NONE',  ( 0.000000000000000000, 0.000000000000000000, 1.000000000000000000 ) ) ;
#12168 = DIRECTION ( 'NONE',  ( 0.000000000000000000, 0.000000000000000000, 1.000000000000000000 ) ) ;
#12169 = DIRECTION ( 'NONE',  ( 0.000000000000000000, 0.000000000000000000, 1.000000000000000000 ) ) ;
#12170 = ORIENTED_EDGE ( 'NONE', *, *, #10950, .F. ) ;
#12171 = VECTOR ( 'NONE', #8683, 999.9999999999998863 ) ;
#12172 = FACE_OUTER_BOUND ( 'NONE', #12385, .T. ) ;
#12173 = EDGE_CURVE ( 'NONE', #637, #5181, #10620, .T. ) ;
#12174 = CARTESIAN_POINT ( 'NONE',  ( 3.764018802651051487, 53.30721710162806204, 24.71610890024348350 ) ) ;
#12175 = CARTESIAN_POINT ( 'NONE',  ( 39.77500000054621410, 22.36655054427230027, 98.07665518445361386 ) ) ;
#12176 = CARTESIAN_POINT ( 'NONE',  ( 26.17500000054623044, 13.07298590277314254, 93.04388485072563242 ) ) ;
#12177 = CARTESIAN_POINT ( 'NONE',  ( 6.629305964221016367, 12.51308527848402896, 90.28034961326086716 ) ) ;
#12178 = CARTESIAN_POINT ( 'NONE',  ( -50.00000000000001421, 0.000000000000000000, 169.9999999999999716 ) ) ;
#12179 = APPLICATION_CONTEXT ( 'automotive_design' ) ;
#12180 = EDGE_CURVE ( 'NONE', #10115, #8484, #7595, .T. ) ;
#12181 = CARTESIAN_POINT ( 'NONE',  ( 35.39999999999998437, 27.13292387221364876, 88.47553407664153724 ) ) ;
#12182 = CARTESIAN_POINT ( 'NONE',  ( 31.49999999999997868, 27.88596668178699645, 90.79316153445363113 ) ) ;
#12183 = ORIENTED_EDGE ( 'NONE', *, *, #9402, .T. ) ;
#12184 = CIRCLE ( 'NONE', #6701, 4.057500000000000107 ) ;
#12185 = LINE ( 'NONE', #3605, #8929 ) ;
#12186 = ORIENTED_EDGE ( 'NONE', *, *, #5900, .T. ) ;
#12187 = DIRECTION ( 'NONE',  ( 0.000000000000000000, 0.000000000000000000, -1.000000000000000000 ) ) ;
#12188 = CARTESIAN_POINT ( 'NONE',  ( 0.000000000000000000, 0.000000000000000000, 0.000000000000000000 ) ) ;
#12189 = CARTESIAN_POINT ( 'NONE',  ( 30.67500000054622333, 15.71886984736413773, 84.90069139318163138 ) ) ;
#12190 = CARTESIAN_POINT ( 'NONE',  ( -3.055901411439527759, 53.97113769530668037, -27.83409950995805460 ) ) ;
#12191 = CARTESIAN_POINT ( 'NONE',  ( 43.27500000054622831, 27.65831843345427998, 90.79316153445363113 ) ) ;
#12192 = CARTESIAN_POINT ( 'NONE',  ( 34.49999999999998579, 12.11403331821300533, 90.79316153445363113 ) ) ;
#12193 = EDGE_CURVE ( 'NONE', #1317, #4704, #997, .T. ) ;
#12194 = LINE ( 'NONE', #3614, #6662 ) ;
#12195 = CARTESIAN_POINT ( 'NONE',  ( 38.97500000054622404, 24.28113015263587471, 84.90069139318163138 ) ) ;
#12196 = ORIENTED_EDGE ( 'NONE', *, *, #5914, .T. ) ;
#12197 = CARTESIAN_POINT ( 'NONE',  ( 45.77500000054622831, 20.00000000000000355, 98.07665518445361386 ) ) ;
#12198 = CARTESIAN_POINT ( 'NONE',  ( 6.000000000000000000, -4.379923479639802331, -2.528749999999993836 ) ) ;
#12199 = ORIENTED_EDGE ( 'NONE', *, *, #9618, .F. ) ;
#12200 = CARTESIAN_POINT ( 'NONE',  ( -5.841425570445385240, 28.12298897545994336, 27.38527483001175611 ) ) ;
#12201 = ORIENTED_EDGE ( 'NONE', *, *, #7535, .T. ) ;
#12202 = EDGE_CURVE ( 'NONE', #6557, #8599, #2651, .T. ) ;
#12203 = CARTESIAN_POINT ( 'NONE',  ( -31.74999999999995737, 0.000000000000000000, 0.000000000000000000 ) ) ;
#12204 = CARTESIAN_POINT ( 'NONE',  ( 6.000000000000000000, -2.919948986426523341, 5.057500000000002771 ) ) ;
#12205 = LINE ( 'NONE', #2492, #10891 ) ;
#12206 = CARTESIAN_POINT ( 'NONE',  ( 31.75000000109246656, 17.56310227825320425, 98.29316153445363113 ) ) ;
#12207 = CARTESIAN_POINT ( 'NONE',  ( 21.27500000054622831, 27.65831843345427998, 90.79316153445363113 ) ) ;
#12208 = CARTESIAN_POINT ( 'NONE',  ( 27.27500000054622475, 26.92701409722686634, 88.54243821818162985 ) ) ;
#12209 = DIRECTION ( 'NONE',  ( 1.000000000000000000, 0.000000000000000000, 0.000000000000000000 ) ) ;
#12210 = LINE ( 'NONE', #11442, #11922 ) ;
#12211 = VERTEX_POINT ( 'NONE', #11394 ) ;
#12212 = CARTESIAN_POINT ( 'NONE',  ( 42.15000000109246514, 12.11403331821300533, 90.79316153445363113 ) ) ;
#12213 =( NAMED_UNIT ( * ) PLANE_ANGLE_UNIT ( ) SI_UNIT ( $, .RADIAN. ) );
#12214 = ORIENTED_EDGE ( 'NONE', *, *, #2850, .F. ) ;
#12215 = CARTESIAN_POINT ( 'NONE',  ( 47.29999999999997584, 26.37988106264029398, 86.15790661882942914 ) ) ;
#12216 = VERTEX_POINT ( 'NONE', #9499 ) ;
#12217 = CARTESIAN_POINT ( 'NONE',  ( 9.999999999999991118, 20.00000000000000355, 197.9999999999999716 ) ) ;
#12218 = CARTESIAN_POINT ( 'NONE',  ( -31.74999999999995737, 0.000000000000000000, 9.000000000000000000 ) ) ;
#12219 = CIRCLE ( 'NONE', #2901, 9.000000000000000000 ) ;
#12220 = CARTESIAN_POINT ( 'NONE',  ( 0.000000000000000000, 139.9999999999999716, -25.00000000000000000 ) ) ;
#12221 = DIRECTION ( 'NONE',  ( 0.000000000000000000, 0.8660254037844380415, -0.5000000000000009992 ) ) ;
#12222 = ADVANCED_FACE ( 'NONE', ( #5566 ), #8004, .T. ) ;
#12223 = FACE_OUTER_BOUND ( 'NONE', #9630, .T. ) ;
#12224 = CARTESIAN_POINT ( 'NONE',  ( -3.567631371761228909, 10.65224600664762455, 20.69704057926737661 ) ) ;
#12225 = DIRECTION ( 'NONE',  ( -1.000000000000000000, -0.000000000000000000, -0.000000000000000000 ) ) ;
#12226 = CARTESIAN_POINT ( 'NONE',  ( 27.47500000054622404, 26.19570976099943493, 95.29460816699764791 ) ) ;
#12227 = CARTESIAN_POINT ( 'NONE',  ( 12.59999999999999964, 0.000000000000000000, 0.000000000000000000 ) ) ;
#12228 = AXIS2_PLACEMENT_3D ( 'NONE', #8358, #6448, #6205 ) ;
#12229 = CARTESIAN_POINT ( 'NONE',  ( 6.000000000000000000, 5.839897972853065333, -6.938893903907228378E-15 ) ) ;
#12230 = VERTEX_POINT ( 'NONE', #1933 ) ;
#12231 = AXIS2_PLACEMENT_3D ( 'NONE', #1351, #5217, #9087 ) ;
#12232 = CARTESIAN_POINT ( 'NONE',  ( 5.000000000000000000, 49.66865400565588828, 24.49489742783178414 ) ) ;
#12233 = CARTESIAN_POINT ( 'NONE',  ( -50.00000000000001421, 22.00000000000000000, 188.4007504869563263 ) ) ;
#12234 = CARTESIAN_POINT ( 'NONE',  ( 39.87500000054622262, 17.63344945572769973, 98.07665518445361386 ) ) ;
#12235 = CARTESIAN_POINT ( 'NONE',  ( 35.47500000054622404, 26.92701409722686634, 93.04388485072563242 ) ) ;
#12236 = VECTOR ( 'NONE', #2683, 1000.000000000000000 ) ;
#12237 = CARTESIAN_POINT ( 'NONE',  ( 29.57500000054622546, 24.28113015263587116, 96.68563167572563088 ) ) ;
#12238 = ADVANCED_FACE ( 'NONE', ( #9623 ), #1809, .T. ) ;
#12239 = CARTESIAN_POINT ( 'NONE',  ( 8.963427797786382101, 15.55435157282535741, -23.33847234685102379 ) ) ;
#12240 = LINE ( 'NONE', #11284, #6629 ) ;
#12241 = AXIS2_PLACEMENT_3D ( 'NONE', #3422, #2842, #5582 ) ;
#12242 = DIRECTION ( 'NONE',  ( 0.000000000000000000, -0.8660254037844395958, -0.4999999999999985012 ) ) ;
#12243 = ORIENTED_EDGE ( 'NONE', *, *, #4750, .F. ) ;
#12244 = EDGE_CURVE ( 'NONE', #2831, #10486, #3708, .T. ) ;
#12245 = CARTESIAN_POINT ( 'NONE',  ( 10.00000000000000355, 20.00000000000000355, 22.91287847477919826 ) ) ;
#12246 = ORIENTED_EDGE ( 'NONE', *, *, #2857, .F. ) ;
#12247 = PLANE ( 'NONE',  #9694 ) ;
#12248 = CARTESIAN_POINT ( 'NONE',  ( 34.87500000054622262, 20.00000000000000355, 83.50966788445364841 ) ) ;
#12249 = CARTESIAN_POINT ( 'NONE',  ( 0.000000000000000000, 0.000000000000000000, 8.400000000000000355 ) ) ;
#12250 = CARTESIAN_POINT ( 'NONE',  ( 48.57500000054623257, 15.71886984736413773, 84.90069139318163138 ) ) ;
#12251 = CARTESIAN_POINT ( 'NONE',  ( 33.27500000054622831, 26.92701409722686634, 88.54243821818162985 ) ) ;
#12252 = CARTESIAN_POINT ( 'NONE',  ( 30.39999999999998792, 12.86707612778636012, 93.11078899226572503 ) ) ;
#12253 = B_SPLINE_CURVE_WITH_KNOTS ( 'NONE', 3,
 ( #7019, #7139, #6256, #6075, #5247, #10957, #7079, #5313, #5062, #368, #10892, #10820, #11845, #3279, #3217, #7912, #8925, #4289, #1194, #6951, #8166, #2133, #11015, #6194, #4231, #242 ),
 .UNSPECIFIED., .F., .F.,
 ( 4, 2, 2, 2, 2, 2, 2, 2, 2, 2, 2, 2, 4 ),
 ( 0.01580552869034228605, 0.01679261472842853362, 0.01777970076651477771, 0.01975387284268728671, 0.02172804491885978878, 0.02271513095694604328, 0.02370221699503229779, 0.02567638907120481373, 0.02666347510929107170, 0.02765056114737732967, 0.02962473322354984562, 0.03061181926163610706, 0.03159890529972236156 ),
 .UNSPECIFIED. ) ;
#12254 = CARTESIAN_POINT ( 'NONE',  ( -7.296251494991419229, 26.84606392143152220, 19.69323068918331288 ) ) ;
#12255 = CARTESIAN_POINT ( 'NONE',  ( 37.27500000054622831, 27.65831843345427998, 90.79316153445363113 ) ) ;
#12256 = ORIENTED_EDGE ( 'NONE', *, *, #11210, .T. ) ;
#12257 = EDGE_CURVE ( 'NONE', #9626, #1347, #5373, .T. ) ;
#12258 = CARTESIAN_POINT ( 'NONE',  ( 47.07500000054622546, 26.19570976099943493, 86.29171490190961435 ) ) ;
#12259 = CARTESIAN_POINT ( 'NONE',  ( -2.510602112304970213, 45.66379892316987821, -20.85116850286192403 ) ) ;
#12260 = ORIENTED_EDGE ( 'NONE', *, *, #2341, .T. ) ;
#12261 = VECTOR ( 'NONE', #10812, 1000.000000000000000 ) ;
#12262 = CARTESIAN_POINT ( 'NONE',  ( 3.252657063245354863, 10.53797398869742352, 20.74903557764927697 ) ) ;
#12263 = VERTEX_POINT ( 'NONE', #8601 ) ;
#12264 = CARTESIAN_POINT ( 'NONE',  ( 42.55000000109246372, 17.56310227825321491, 83.29316153445364534 ) ) ;
#12265 = CARTESIAN_POINT ( 'NONE',  ( -50.00000000000001421, 92.00000000000000000, 166.8533255156881694 ) ) ;
#12266 = EDGE_CURVE ( 'NONE', #10006, #9751, #303, .T. ) ;
#12267 = CARTESIAN_POINT ( 'NONE',  ( -31.74999999999995737, 0.000000000000000000, 0.000000000000000000 ) ) ;
#12268 = AXIS2_PLACEMENT_3D ( 'NONE', #6637, #6768, #3719 ) ;
#12269 = DIRECTION ( 'NONE',  ( 0.000000000000000000, 0.000000000000000000, 1.000000000000000000 ) ) ;
#12270 = VECTOR ( 'NONE', #10952, 1000.000000000000000 ) ;
#12271 = CARTESIAN_POINT ( 'NONE',  ( 25.57500000054622546, 24.28113015263587116, 96.68563167572563088 ) ) ;
#12272 = CARTESIAN_POINT ( 'NONE',  ( 26.87500000054622618, 20.00000000000000355, 83.50966788445364841 ) ) ;
#12273 = CARTESIAN_POINT ( 'NONE',  ( 41.39999999999999147, 27.13292387221364876, 88.47553407664153724 ) ) ;
#12274 = EDGE_CURVE ( 'NONE', #12014, #8987, #12471, .T. ) ;
#12275 = CARTESIAN_POINT ( 'NONE',  ( -2.505953076466797658, 45.67021871533034982, 24.87450930309000441 ) ) ;
#12276 = EDGE_LOOP ( 'NONE', ( #7831, #5868, #2891, #4317 ) ) ;
#12277 = VECTOR ( 'NONE', #1508, 1000.000000000000000 ) ;
#12278 = CARTESIAN_POINT ( 'NONE',  ( 35.85000000109246798, 15.59161060780645691, 96.86078899226572503 ) ) ;
#12279 = CARTESIAN_POINT ( 'NONE',  ( 24.79999999999999005, 15.59161060780646046, 84.72553407664153724 ) ) ;
#12280 = ORIENTED_EDGE ( 'NONE', *, *, #10783, .T. ) ;
#12281 = CARTESIAN_POINT ( 'NONE',  ( 47.89999999999997726, 22.43689772174681707, 98.29316153445361692 ) ) ;
#12282 = EDGE_LOOP ( 'NONE', ( #3259, #10000, #5213, #351, #3069 ) ) ;
#12283 = AXIS2_PLACEMENT_3D ( 'NONE', #4162, #11907, #173 ) ;
#12284 = CARTESIAN_POINT ( 'NONE',  ( 0.3297592447147374983, 55.00000000000001421, 21.00000000000000711 ) ) ;
#12285 = CARTESIAN_POINT ( 'NONE',  ( 3.061616997868383043E-15, 0.000000000000000000, 25.00000000000000000 ) ) ;
#12286 = CARTESIAN_POINT ( 'NONE',  ( 0.000000000000000000, 20.00000000000000355, -28.00000000000000711 ) ) ;
#12287 = CARTESIAN_POINT ( 'NONE',  ( 27.69999999999998508, 26.37988106264029398, 95.42841645007781892 ) ) ;
#12288 = CARTESIAN_POINT ( 'NONE',  ( -9.935036394566825635, 18.68123011217310392, 18.50181441894565637 ) ) ;
#12289 = CYLINDRICAL_SURFACE ( 'NONE', #4116, 10.00000000000000355 ) ;
#12290 = CARTESIAN_POINT ( 'NONE',  ( 20.97500000054622760, 24.28113015263587471, 84.90069139318163138 ) ) ;
#12291 = CARTESIAN_POINT ( 'NONE',  ( 7.931687869515056555, 26.09867752937626406, 23.70939416258605803 ) ) ;
#12292 = CARTESIAN_POINT ( 'NONE',  ( 3.061565168526138680E-15, 55.00000000000000000, 25.00000000000000000 ) ) ;
#12293 = ORIENTED_EDGE ( 'NONE', *, *, #7144, .T. ) ;
#12294 = CIRCLE ( 'NONE', #3377, 6.599999999999998757 ) ;
#12295 = DIRECTION ( 'NONE',  ( 0.000000000000000000, 0.000000000000000000, 1.000000000000000000 ) ) ;
#12296 = DIRECTION ( 'NONE',  ( 1.000000000000000000, 0.000000000000000000, 0.000000000000000000 ) ) ;
#12297 = CARTESIAN_POINT ( 'NONE',  ( 34.67500000054621268, 17.63344945572770328, 83.50966788445364841 ) ) ;
#12298 = CARTESIAN_POINT ( 'NONE',  ( 37.87500000054622262, 20.00000000000000355, 98.07665518445361386 ) ) ;
#12299 = AXIS2_PLACEMENT_3D ( 'NONE', #5515, #6578, #10442 ) ;
#12300 = LINE ( 'NONE', #3599, #5381 ) ;
#12301 = FACE_OUTER_BOUND ( 'NONE', #10245, .T. ) ;
#12302 = CARTESIAN_POINT ( 'NONE',  ( 5.000000000000000000, 49.66865400565588828, 24.49489742783178414 ) ) ;
#12303 = CARTESIAN_POINT ( 'NONE',  ( -36.00000000000001421, 77.00000000000000000, 154.3533255156881978 ) ) ;
#12304 = DIRECTION ( 'NONE',  ( -1.000000000000000000, 0.000000000000000000, 0.000000000000000000 ) ) ;
#12305 = ORIENTED_EDGE ( 'NONE', *, *, #11312, .F. ) ;
#12306 = CARTESIAN_POINT ( 'NONE',  ( 5.340684424226280325E-17, 55.00000000000000000, -25.00000000000000000 ) ) ;
#12307 = AXIS2_PLACEMENT_3D ( 'NONE', #1181, #1055, #2185 ) ;
#12308 = EDGE_CURVE ( 'NONE', #6176, #6737, #738, .T. ) ;
#12309 = CARTESIAN_POINT ( 'NONE',  ( 25.77500000054622475, 22.36655054427230027, 98.07665518445361386 ) ) ;
#12310 = CARTESIAN_POINT ( 'NONE',  ( 28.75000000109245946, 22.43689772174679575, 83.29316153445363113 ) ) ;
#12312 = CARTESIAN_POINT ( 'NONE',  ( 47.57500000054622546, 24.28113015263587116, 96.68563167572563088 ) ) ;
#12311 = ADVANCED_BREP_SHAPE_REPRESENTATION ( '', ( #2064, #9021 ), #5775 ) ;
#12313 = CARTESIAN_POINT ( 'NONE',  ( 26.37500000054622618, 12.34168156654572535, 90.79316153445363113 ) ) ;
#12314 = CARTESIAN_POINT ( 'NONE',  ( 27.39999999999998792, 27.13292387221364876, 88.47553407664153724 ) ) ;
#12315 = CARTESIAN_POINT ( 'NONE',  ( 9.657343816332662811, 22.61594140643868300, 23.05962942824199757 ) ) ;
#12316 = CARTESIAN_POINT ( 'NONE',  ( 36.47500000054622404, 13.80429023900056684, 86.29171490190961435 ) ) ;
#12317 = ORIENTED_EDGE ( 'NONE', *, *, #3157, .T. ) ;
#12318 = CARTESIAN_POINT ( 'NONE',  ( 48.77500000054622831, 20.00000000000000355, 83.50966788445364841 ) ) ;
#12319 = CARTESIAN_POINT ( 'NONE',  ( 6.000000000000000000, 0.000000000000000000, 0.000000000000000000 ) ) ;
#12320 = VERTEX_POINT ( 'NONE', #7375 ) ;
#12321 = DIRECTION ( 'NONE',  ( 0.000000000000000000, 0.000000000000000000, -1.000000000000000000 ) ) ;
#12322 = ORIENTED_EDGE ( 'NONE', *, *, #4904, .F. ) ;
#12323 = CARTESIAN_POINT ( 'NONE',  ( 7.532348232781783892, 26.60942912475959332, -23.84307605514715434 ) ) ;
#12324 = VECTOR ( 'NONE', #7154, 1000.000000000000000 ) ;
#12325 = DIRECTION ( 'NONE',  ( 1.000000000000000000, 0.000000000000000000, 0.000000000000000000 ) ) ;
#12326 = PLANE ( 'NONE',  #3796 ) ;
#12327 = VECTOR ( 'NONE', #9115, 1000.000000000000000 ) ;
#12328 = DIRECTION ( 'NONE',  ( -1.000000000000000000, 0.000000000000000000, 0.000000000000000000 ) ) ;
#12329 = ADVANCED_FACE ( 'NONE', ( #4334 ), #1427, .T. ) ;
#12330 = CARTESIAN_POINT ( 'NONE',  ( 24.97500000054622760, 24.28113015263587471, 84.90069139318163138 ) ) ;
#12331 = CARTESIAN_POINT ( 'NONE',  ( 20.37500000054621907, 12.34168156654572535, 90.79316153445363113 ) ) ;
#12332 = CARTESIAN_POINT ( 'NONE',  ( 27.49999999999999645, 20.00000000000000355, 171.0000000000000000 ) ) ;
#12333 =( BOUNDED_CURVE ( )  B_SPLINE_CURVE ( 2, ( #1405, #4561, #9204, #3544, #5270, #12182, #11287, #7351, #6402, #10267, #2350 ),
 .UNSPECIFIED., .F., .F. ) 
 B_SPLINE_CURVE_WITH_KNOTS ( ( 3, 2, 2, 2, 2, 3 ),
 ( 0.5999999999999999778, 0.6066666666666666874, 0.6133333333333332860, 0.6199999999999999956, 0.6266666666666667052, 0.6333333333333333037 ),
 .UNSPECIFIED. ) 
 CURVE ( )  GEOMETRIC_REPRESENTATION_ITEM ( )  RATIONAL_B_SPLINE_CURVE ( ( 1.000000000000000000, 0.9510565162951535312, 1.000000000000000000, 0.9510565162951535312, 1.000000000000000000, 0.9510565162951535312, 1.000000000000000000, 0.9510565162951535312, 1.000000000000000000, 0.9510565162951535312, 1.000000000000000000 ) ) 
 REPRESENTATION_ITEM ( '' )  );
#12334 = CARTESIAN_POINT ( 'NONE',  ( -4.744071016079746350, 48.38731143956220393, 24.54607980264442091 ) ) ;
#12335 = VECTOR ( 'NONE', #4814, 999.9999999999998863 ) ;
#12336 = VERTEX_POINT ( 'NONE', #7911 ) ;
#12337 = CARTESIAN_POINT ( 'NONE',  ( 38.05000000109246372, 12.86707612778636012, 93.11078899226572503 ) ) ;
#12338 = CARTESIAN_POINT ( 'NONE',  ( 24.69999999999998508, 13.62011893735970958, 86.15790661882942914 ) ) ;
#12339 = ORIENTED_EDGE ( 'NONE', *, *, #8600, .T. ) ;
#12340 = CARTESIAN_POINT ( 'NONE',  ( -36.00000000000001421, 77.00000000000000000, 166.8533255156881694 ) ) ;
#12341 = ORIENTED_EDGE ( 'NONE', *, *, #8808, .F. ) ;
#12342 = CARTESIAN_POINT ( 'NONE',  ( 4.490845867985273188, 52.22224976665338403, 20.51459889515917467 ) ) ;
#12343 = CARTESIAN_POINT ( 'NONE',  ( -0.3313438815916917579, 54.99999999999998579, -25.00000000000000000 ) ) ;
#12344 = EDGE_CURVE ( 'NONE', #7546, #3410, #8271, .T. ) ;
#12345 = LINE ( 'NONE', #6502, #3712 ) ;
#12346 = CARTESIAN_POINT ( 'NONE',  ( 41.35889894354065177, 20.00000000000000355, 172.0000000000000000 ) ) ;
#12347 = DIRECTION ( 'NONE',  ( 0.000000000000000000, -1.000000000000000000, 0.000000000000000000 ) ) ;
#12348 = EDGE_LOOP ( 'NONE', ( #5866, #8221, #9755, #6691, #3348 ) ) ;
#12349 = DIRECTION ( 'NONE',  ( 0.000000000000000000, 0.000000000000000000, -1.000000000000000000 ) ) ;
#12350 = EDGE_CURVE ( 'NONE', #10641, #10590, #7335, .T. ) ;
#12351 = DIRECTION ( 'NONE',  ( 1.000000000000000000, 0.000000000000000000, 0.000000000000000000 ) ) ;
#12352 = CARTESIAN_POINT ( 'NONE',  ( 19.87500000054622973, 17.63344945572769973, 98.07665518445361386 ) ) ;
#12353 = PLANE ( 'NONE',  #9244 ) ;
#12354 = CARTESIAN_POINT ( 'NONE',  ( -0.3301821175306443035, 55.00000000000001421, 25.00000000000000000 ) ) ;
#12355 = VERTEX_POINT ( 'NONE', #12141 ) ;
#12356 = ORIENTED_EDGE ( 'NONE', *, *, #7359, .T. ) ;
#12357 = EDGE_CURVE ( 'NONE', #1279, #6113, #9882, .T. ) ;
#12358 = CARTESIAN_POINT ( 'NONE',  ( 6.000000000000000000, -2.919948986426538440, -5.057499999999997442 ) ) ;
#12359 = VECTOR ( 'NONE', #5988, 1000.000000000000114 ) ;
#12360 = CARTESIAN_POINT ( 'NONE',  ( 0.000000000000000000, 0.000000000000000000, -28.00000000000000355 ) ) ;
#12361 = CARTESIAN_POINT ( 'NONE',  ( 38.97500000054623115, 22.36655054427230382, 83.50966788445364841 ) ) ;
#12362 = CARTESIAN_POINT ( 'NONE',  ( 21.37500000054622618, 26.92701409722686634, 93.04388485072563242 ) ) ;
#12363 = CARTESIAN_POINT ( 'NONE',  ( 1.500000000000001332, 0.000000000000000000, 8.000000000000000000 ) ) ;
#12364 = CARTESIAN_POINT ( 'NONE',  ( 3.764226701178052803, 46.69296989397847852, 24.71608072572789538 ) ) ;
#12365 = CARTESIAN_POINT ( 'NONE',  ( 0.000000000000000000, 2.342598717236912265, 4.057499999999998330 ) ) ;
#12366 = CARTESIAN_POINT ( 'NONE',  ( 3.061565168526138680E-15, 55.00000000000000000, 25.00000000000000000 ) ) ;
#12367 = CARTESIAN_POINT ( 'NONE',  ( 121.9999999999999858, 0.000000000000000000, 0.000000000000000000 ) ) ;
#12368 = VERTEX_POINT ( 'NONE', #4394 ) ;
#12369 = EDGE_CURVE ( 'NONE', #11432, #2307, #5356, .T. ) ;
#12370 = AXIS2_PLACEMENT_3D ( 'NONE', #2455, #11274, #12169 ) ;
#12371 = LINE ( 'NONE', #2783, #7258 ) ;
#12372 = DIRECTION ( 'NONE',  ( 0.000000000000000000, 0.000000000000000000, -1.000000000000000000 ) ) ;
#12373 = CARTESIAN_POINT ( 'NONE',  ( 26.67500000054622333, 15.71886984736413773, 84.90069139318163138 ) ) ;
#12374 = CARTESIAN_POINT ( 'NONE',  ( 29.65000000109246514, 20.00000000000000355, 98.29316153445363113 ) ) ;
#12375 = CARTESIAN_POINT ( 'NONE',  ( 40.97500000054622404, 24.28113015263587471, 84.90069139318163138 ) ) ;
#12376 = CARTESIAN_POINT ( 'NONE',  ( 28.77500000054622831, 17.63344945572770328, 83.50966788445364841 ) ) ;
#12377 = CARTESIAN_POINT ( 'NONE',  ( 30.79999999999998650, 15.59161060780646046, 84.72553407664153724 ) ) ;
#12378 = AXIS2_PLACEMENT_3D ( 'NONE', #1349, #4316, #10096 ) ;
#12379 = CARTESIAN_POINT ( 'NONE',  ( 30.49999999999998934, 12.11403331821300533, 90.79316153445363113 ) ) ;
#12380 = ADVANCED_FACE ( 'NONE', ( #1193, #3381 ), #11244, .T. ) ;
#12381 = CARTESIAN_POINT ( 'NONE',  ( 37.77500000054623541, 20.00000000000000355, 98.07665518445361386 ) ) ;
#12382 = EDGE_LOOP ( 'NONE', ( #8303, #7164 ) ) ;
#12383 = CARTESIAN_POINT ( 'NONE',  ( 21.05000000109246727, 27.13292387221364876, 88.47553407664153724 ) ) ;
#12384 = CARTESIAN_POINT ( 'NONE',  ( -2.217721585883460023, 45.50683808975505684, -20.88476930822203315 ) ) ;
#12385 = EDGE_LOOP ( 'NONE', ( #11384, #1904 ) ) ;
#12386 = CARTESIAN_POINT ( 'NONE',  ( -50.00000000000001421, 84.49999999999998579, 146.8533255156881978 ) ) ;
#12387 = ORIENTED_EDGE ( 'NONE', *, *, #3620, .T. ) ;
#12388 = LINE ( 'NONE', #1845, #11440 ) ;
#12389 = CARTESIAN_POINT ( 'NONE',  ( 43.99999999999999289, 20.00000000000000355, 98.29316153445363113 ) ) ;
#12390 = DIRECTION ( 'NONE',  ( 0.000000000000000000, 1.000000000000000000, -1.039664082171044481E-15 ) ) ;
#12391 = CARTESIAN_POINT ( 'NONE',  ( 42.27500000054622120, 13.07298590277314254, 93.04388485072563242 ) ) ;
#12392 = DIRECTION ( 'NONE',  ( 0.000000000000000000, 0.000000000000000000, -1.000000000000000000 ) ) ;
#12393 = CARTESIAN_POINT ( 'NONE',  ( 21.57500000054622546, 26.19570976099943493, 95.29460816699764791 ) ) ;
#12394 = DIRECTION ( 'NONE',  ( -0.000000000000000000, -0.000000000000000000, 1.000000000000000000 ) ) ;
#12395 = LINE ( 'NONE', #11252, #177 ) ;
#12396 = ORIENTED_EDGE ( 'NONE', *, *, #2398, .T. ) ;
#12397 = CARTESIAN_POINT ( 'NONE',  ( 40.65000000109246514, 20.00000000000000355, 83.29316153445364534 ) ) ;
#12398 = DIRECTION ( 'NONE',  ( -0.000000000000000000, 0.7071067811865511255, 0.7071067811865440200 ) ) ;
#12399 = ORIENTED_EDGE ( 'NONE', *, *, #5893, .T. ) ;
#12400 = LINE ( 'NONE', #10607, #10837 ) ;
#12401 = EDGE_CURVE ( 'NONE', #8586, #10504, #6009, .T. ) ;
#12402 = VERTEX_POINT ( 'NONE', #8858 ) ;
#12403 = CARTESIAN_POINT ( 'NONE',  ( -2.000000000000015543, 20.00000000000000355, 83.29316153445364534 ) ) ;
#12404 = CARTESIAN_POINT ( 'NONE',  ( 30.85000000109246443, 24.40838939219355197, 84.72553407664153724 ) ) ;
#12405 = DIRECTION ( 'NONE',  ( 1.000000000000000000, -0.000000000000000000, -0.000000000000000000 ) ) ;
#12406 =( BOUNDED_CURVE ( )  B_SPLINE_CURVE ( 2, ( #8675, #1009, #4613, #8735, #11593, #1751, #48, #3911, #11528, #10694, #8551 ),
 .UNSPECIFIED., .F., .F. ) 
 B_SPLINE_CURVE_WITH_KNOTS ( ( 3, 2, 2, 2, 2, 3 ),
 ( 0.1999999999999999278, 0.2066666666666665819, 0.2133333333333332915, 0.2199999999999999456, 0.2266666666666666274, 0.2333333333333333093 ),
 .UNSPECIFIED. ) 
 CURVE ( )  GEOMETRIC_REPRESENTATION_ITEM ( )  RATIONAL_B_SPLINE_CURVE ( ( 1.000000000000000666, 0.9510565162951528650, 1.000000000000000000, 0.9510565162951535312, 1.000000000000000000, 0.9510565162951535312, 1.000000000000000000, 0.9510565162951535312, 1.000000000000000000, 0.9510565162951537532, 0.9999999999999997780 ) ) 
 REPRESENTATION_ITEM ( '' )  );
#12407 = DIRECTION ( 'NONE',  ( -0.000000000000000000, -1.000000000000000000, -0.000000000000000000 ) ) ;
#12408 = CARTESIAN_POINT ( 'NONE',  ( -3.051733061893640908, 46.02601656636597482, 20.77886321925161894 ) ) ;
#12409 = ORIENTED_EDGE ( 'NONE', *, *, #737, .F. ) ;
#12410 = CARTESIAN_POINT ( 'NONE',  ( 0.3311574161024399277, 54.99999999999999289, -28.00000000000000000 ) ) ;
#12411 = DIRECTION ( 'NONE',  ( -1.000000000000000000, 0.000000000000000000, 0.000000000000000000 ) ) ;
#12412 = CARTESIAN_POINT ( 'NONE',  ( 23.47500000054623115, 26.19570976099943493, 95.29460816699764791 ) ) ;
#12413 = DIRECTION ( 'NONE',  ( 1.000000000000000000, 0.000000000000000000, 0.000000000000000000 ) ) ;
#12414 = DIRECTION ( 'NONE',  ( 0.000000000000000000, 0.8660254037844380415, -0.5000000000000012212 ) ) ;
#12415 = ORIENTED_EDGE ( 'NONE', *, *, #9869, .F. ) ;
#12416 = VERTEX_POINT ( 'NONE', #2489 ) ;
#12417 = VECTOR ( 'NONE', #9214, 1000.000000000000000 ) ;
#12418 = CYLINDRICAL_SURFACE ( 'NONE', #10868, 7.499999999999978684 ) ;
#12419 = ADVANCED_FACE ( 'NONE', ( #11778 ), #533, .F. ) ;
#12420 = CARTESIAN_POINT ( 'NONE',  ( -50.00000000000001421, 20.00000000000000000, 137.5000000000000000 ) ) ;
#12421 = DIRECTION ( 'NONE',  ( 0.000000000000000000, 0.4999999999999987232, -0.8660254037844392627 ) ) ;
#12422 = CARTESIAN_POINT ( 'NONE',  ( 28.65000000109246514, 20.00000000000000355, 83.29316153445364534 ) ) ;
#12423 = EDGE_CURVE ( 'NONE', #6252, #1936, #6306, .T. ) ;
#12424 = AXIS2_PLACEMENT_3D ( 'NONE', #6390, #7212, #555 ) ;
#12425 = CARTESIAN_POINT ( 'NONE',  ( 0.000000000000000000, 20.00000000000000355, -28.00000000000000711 ) ) ;
#12426 = CARTESIAN_POINT ( 'NONE',  ( 10.00000000000000355, 20.00000000000000355, -22.91287847477919826 ) ) ;
#12427 = EDGE_CURVE ( 'NONE', #1672, #10006, #7018, .T. ) ;
#12428 = CARTESIAN_POINT ( 'NONE',  ( -50.00000000000001421, 18.00000000000000355, 152.2284161474004520 ) ) ;
#12429 = DIRECTION ( 'NONE',  ( 0.000000000000000000, 0.000000000000000000, 1.000000000000000000 ) ) ;
#12430 = EDGE_LOOP ( 'NONE', ( #9082, #8330, #11921, #6977, #11556, #12256 ) ) ;
#12431 = DIRECTION ( 'NONE',  ( 0.000000000000000000, 0.000000000000000000, -1.000000000000000000 ) ) ;
#12432 = APPLICATION_PROTOCOL_DEFINITION ( 'draft international standard', 'automotive_design', 1998, #8857 ) ;
#12433 = AXIS2_PLACEMENT_3D ( 'NONE', #6670, #5672, #719 ) ;
#12434 = CARTESIAN_POINT ( 'NONE',  ( 28.57500000054622191, 13.80429023900056684, 86.29171490190961435 ) ) ;
#12435 = CARTESIAN_POINT ( 'NONE',  ( 36.69999999999999574, 13.62011893735970958, 86.15790661882942914 ) ) ;
#12436 = PRODUCT_DEFINITION_FORMATION_WITH_SPECIFIED_SOURCE ( 'ANY', '', #6099, .NOT_KNOWN. ) ;
#12437 = CARTESIAN_POINT ( 'NONE',  ( 36.47500000054622404, 13.80429023900056684, 86.29171490190961435 ) ) ;
#12438 = CARTESIAN_POINT ( 'NONE',  ( 30.07500000054622546, 15.71886984736413417, 96.68563167572563088 ) ) ;
#12439 = CARTESIAN_POINT ( 'NONE',  ( 30.59999999999998721, 12.86707612778636012, 88.47553407664152303 ) ) ;
#12440 = CARTESIAN_POINT ( 'NONE',  ( 29.99999999999998934, 20.00000000000000355, 98.29316153445363113 ) ) ;
#12441 = CARTESIAN_POINT ( 'NONE',  ( 40.17500000054623399, 13.07298590277314254, 93.04388485072563242 ) ) ;
#12442 = ORIENTED_EDGE ( 'NONE', *, *, #10633, .T. ) ;
#12443 = CARTESIAN_POINT ( 'NONE',  ( 47.97500000054622404, 15.71886984736413417, 96.68563167572563088 ) ) ;
#12444 = CARTESIAN_POINT ( 'NONE',  ( -10.00000000000000355, 20.00000000000000355, 18.46618531261938756 ) ) ;
#12445 = ORIENTED_EDGE ( 'NONE', *, *, #4626, .T. ) ;
#12446 = CARTESIAN_POINT ( 'NONE',  ( 9.349263383750175294, 16.43657559142555868, 18.80454793984171147 ) ) ;
#12447 = ORIENTED_EDGE ( 'NONE', *, *, #8947, .T. ) ;
#12448 = CARTESIAN_POINT ( 'NONE',  ( 41.95000000109246230, 13.62011893735970958, 95.42841645007781892 ) ) ;
#12449 = DIRECTION ( 'NONE',  ( 0.000000000000000000, 1.000000000000000000, 0.000000000000000000 ) ) ;
#12450 = CARTESIAN_POINT ( 'NONE',  ( 3.061616998149962604E-15, 10.00000000000000000, 25.00000000000000000 ) ) ;
#12451 = CARTESIAN_POINT ( 'NONE',  ( 46.37500000054621552, 12.34168156654572357, 90.79316153445363113 ) ) ;
#12452 = CARTESIAN_POINT ( 'NONE',  ( 20.79999999999999005, 15.59161060780646046, 84.72553407664153724 ) ) ;
#12453 = DIRECTION ( 'NONE',  ( -1.000000000000000000, -0.000000000000000000, -0.000000000000000000 ) ) ;
#12454 = CARTESIAN_POINT ( 'NONE',  ( 46.09999999999998010, 17.56310227825320425, 98.29316153445363113 ) ) ;
#12455 = CARTESIAN_POINT ( 'NONE',  ( 41.29999999999999005, 26.37988106264029398, 86.15790661882942914 ) ) ;
#12456 = LINE ( 'NONE', #9423, #9895 ) ;
#12457 = VERTEX_POINT ( 'NONE', #3084 ) ;
#12458 = CARTESIAN_POINT ( 'NONE',  ( 38.15000000109245804, 12.11403331821300533, 90.79316153445363113 ) ) ;
#12459 = DIRECTION ( 'NONE',  ( 1.000000000000000000, 0.000000000000000000, 0.000000000000000000 ) ) ;
#12460 = EDGE_LOOP ( 'NONE', ( #4915, #6699, #8791, #10606 ) ) ;
#12461 =( LENGTH_UNIT ( ) NAMED_UNIT ( * ) SI_UNIT ( .MILLI., .METRE. ) );
#12462 = VERTEX_POINT ( 'NONE', #6074 ) ;
#12463 = DIRECTION ( 'NONE',  ( 0.000000000000000000, 0.000000000000000000, -1.000000000000000000 ) ) ;
#12464 = CIRCLE ( 'NONE', #5577, 0.5999999999999998668 ) ;
#12465 = ADVANCED_FACE ( 'NONE', ( #10233 ), #1545, .F. ) ;
#12466 = LINE ( 'NONE', #4792, #4327 ) ;
#12467 = VECTOR ( 'NONE', #556, 1000.000000000000000 ) ;
#12468 = DIRECTION ( 'NONE',  ( -1.000000000000000000, -0.000000000000000000, -0.000000000000000000 ) ) ;
#12469 = CARTESIAN_POINT ( 'NONE',  ( 27.79999999999998650, 24.40838939219354842, 96.86078899226572503 ) ) ;
#12470 = ORIENTED_EDGE ( 'NONE', *, *, #10824, .T. ) ;
#12471 = LINE ( 'NONE', #9436, #5166 ) ;
#12472 = DIRECTION ( 'NONE',  ( -0.000000000000000000, 1.000000000000000000, 0.000000000000000000 ) ) ;
#12473 = CARTESIAN_POINT ( 'NONE',  ( 23.07500000054622902, 26.19570976099943493, 86.29171490190961435 ) ) ;
#12474 = ORIENTED_EDGE ( 'NONE', *, *, #18, .F. ) ;
#12475 = FACE_OUTER_BOUND ( 'NONE', #5755, .T. ) ;
#12476 = CARTESIAN_POINT ( 'NONE',  ( 1.620915035299892226, 54.74117664902413338, -20.93952827735066791 ) ) ;
#12477 = ORIENTED_EDGE ( 'NONE', *, *, #4435, .T. ) ;
#12478 = ORIENTED_EDGE ( 'NONE', *, *, #8470, .T. ) ;
#12479 = CARTESIAN_POINT ( 'NONE',  ( -6.616163141694259231, 27.50539512973521283, -19.93225680451049087 ) ) ;
#12480 = CARTESIAN_POINT ( 'NONE',  ( 27.49999999999999645, 20.00000000000000355, 187.9999999999999716 ) ) ;
#12481 = EDGE_CURVE ( 'NONE', #1426, #11516, #3149, .T. ) ;
#12482 = CARTESIAN_POINT ( 'NONE',  ( 22.07500000054622191, 13.80429023900056507, 95.29460816699764791 ) ) ;
#12483 = CARTESIAN_POINT ( 'NONE',  ( 0.3267965066156393039, 44.99999999999999289, -25.00000000000000355 ) ) ;
#12484 = CARTESIAN_POINT ( 'NONE',  ( -4.968127171134807618, 50.65287670289590949, -20.40397231773725650 ) ) ;
#12485 = CARTESIAN_POINT ( 'NONE',  ( -50.00000000000001421, 77.00000000000000000, 146.8533255156881978 ) ) ;
#12486 = AXIS2_PLACEMENT_3D ( 'NONE', #7081, #7021, #9758 ) ;
#12487 = DIRECTION ( 'NONE',  ( 1.000000000000000000, 0.000000000000000000, 0.000000000000000000 ) ) ;
#12488 = CARTESIAN_POINT ( 'NONE',  ( -20.27158385259951956, 18.00000000000000355, 169.9999999999999716 ) ) ;
#12489 = ORIENTED_EDGE ( 'NONE', *, *, #9053, .F. ) ;
#12490 = CARTESIAN_POINT ( 'NONE',  ( 19.99999999999999645, 20.00000000000000355, 99.99999999999997158 ) ) ;
#12491 = SHAPE_DEFINITION_REPRESENTATION ( #117, #10815 ) ;
#12492 = MECHANICAL_DESIGN_GEOMETRIC_PRESENTATION_REPRESENTATION (  '', ( #5415 ), #6225 ) ;
#12493 = CARTESIAN_POINT ( 'NONE',  ( 27.37500000054622262, 27.65831843345427998, 90.79316153445363113 ) ) ;
#12494 = CARTESIAN_POINT ( 'NONE',  ( 12.59999999999999964, 0.000000000000000000, 0.000000000000000000 ) ) ;
#12495 = ADVANCED_FACE ( 'NONE', ( #6950 ), #3503, .T. ) ;
#12496 = CARTESIAN_POINT ( 'NONE',  ( 40.67500000054623399, 17.63344945572770328, 83.50966788445364841 ) ) ;
#12497 = CARTESIAN_POINT ( 'NONE',  ( 25.17500000054622689, 26.19570976099943493, 86.29171490190961435 ) ) ;
#12498 = CARTESIAN_POINT ( 'NONE',  ( 32.49999999999997868, 12.11403331821300533, 90.79316153445363113 ) ) ;
#12499 = CARTESIAN_POINT ( 'NONE',  ( 30.59999999999998721, 12.86707612778636012, 88.47553407664152303 ) ) ;
#12500 = CARTESIAN_POINT ( 'NONE',  ( 32.37500000054622973, 13.07298590277314432, 88.54243821818161564 ) ) ;
#12501 = ORIENTED_EDGE ( 'NONE', *, *, #873, .T. ) ;
#12502 = EDGE_CURVE ( 'NONE', #12216, #7706, #11715, .T. ) ;
#12503 = CARTESIAN_POINT ( 'NONE',  ( -6.999999999999999112, 92.00000000000000000, 69.99999999999998579 ) ) ;
#12504 = AXIS2_PLACEMENT_3D ( 'NONE', #8397, #10413, #1727 ) ;
#12505 = EDGE_LOOP ( 'NONE', ( #8592, #46, #6949, #8985 ) ) ;
#12506 = CARTESIAN_POINT ( 'NONE',  ( 8.663040577955531063, 14.96273206212219975, 19.13393308409949967 ) ) ;
#12507 = EDGE_LOOP ( 'NONE', ( #7279, #3654, #7611 ) ) ;
#12508 = EDGE_CURVE ( 'NONE', #6404, #3714, #8991, .T. ) ;
#12509 = CARTESIAN_POINT ( 'NONE',  ( 9.935507569286025742, 21.31398369048515562, -22.94135581966985526 ) ) ;
#12510 = FACE_OUTER_BOUND ( 'NONE', #9782, .T. ) ;
#12511 = CARTESIAN_POINT ( 'NONE',  ( 0.6583504323226527788, 45.03273075554383098, -27.99410254389716357 ) ) ;
#12512 = CARTESIAN_POINT ( 'NONE',  ( 46.87500000054622262, 20.00000000000000355, 83.50966788445364841 ) ) ;
#12513 = CARTESIAN_POINT ( 'NONE',  ( 27.49999999999999645, 20.00000000000000355, 187.9999999999999716 ) ) ;
#12514 = AXIS2_PLACEMENT_3D ( 'NONE', #6986, #11623, #6918 ) ;
#12515 = CARTESIAN_POINT ( 'NONE',  ( -2.000000000000015543, 20.00000000000000355, 98.29316153445363113 ) ) ;
#12516 = CARTESIAN_POINT ( 'NONE',  ( 46.07500000054622546, 15.71886984736413417, 96.68563167572563088 ) ) ;
#12517 = CARTESIAN_POINT ( 'NONE',  ( 46.49999999999999289, 12.11403331821300533, 90.79316153445363113 ) ) ;
#12518 = CARTESIAN_POINT ( 'NONE',  ( -10.00000000000000355, 20.00000000000000355, -22.91287847477919826 ) ) ;
#12519 = CARTESIAN_POINT ( 'NONE',  ( 49.37500000054622973, 26.92701409722686634, 93.04388485072563242 ) ) ;
#12520 = ORIENTED_EDGE ( 'NONE', *, *, #12274, .F. ) ;
#12521 = CARTESIAN_POINT ( 'NONE',  ( 36.25000000109246656, 12.86707612778636012, 88.47553407664152303 ) ) ;
#12522 = EDGE_LOOP ( 'NONE', ( #7001, #4034, #7967, #8855 ) ) ;
#12523 = PLANE ( 'NONE',  #3540 ) ;
#12524 = ORIENTED_EDGE ( 'NONE', *, *, #243, .F. ) ;
#12525 = CARTESIAN_POINT ( 'NONE',  ( -3.242423582264189807, 29.46551675503955536, -24.79088612835948879 ) ) ;
#12526 = CARTESIAN_POINT ( 'NONE',  ( 8.653685250178629218, 14.97800528606349424, -19.13485699315961597 ) ) ;
#12527 = CARTESIAN_POINT ( 'NONE',  ( 27.49999999999999645, 20.00000000000000355, 189.0000000000000000 ) ) ;
#12528 = TOROIDAL_SURFACE ( 'NONE', #989, 8.400000000000000355, 0.5999999999999999778 ) ;
#12529 = CARTESIAN_POINT ( 'NONE',  ( 37.17500000054622689, 26.92701409722686634, 88.54243821818162985 ) ) ;
#12530 = CARTESIAN_POINT ( 'NONE',  ( 5.000000000000000000, 4.685197434473814759, -5.637851296924623057E-15 ) ) ;
#12531 = CARTESIAN_POINT ( 'NONE',  ( 31.65000000109246514, 20.00000000000000355, 98.29316153445363113 ) ) ;
#12532 = ORIENTED_EDGE ( 'NONE', *, *, #10684, .F. ) ;
#12533 = DIRECTION ( 'NONE',  ( -0.000000000000000000, -0.000000000000000000, 1.000000000000000000 ) ) ;
#12534 = CYLINDRICAL_SURFACE ( 'NONE', #11016, 7.499999999999992895 ) ;
#12535 = CARTESIAN_POINT ( 'NONE',  ( 21.07500000054622546, 26.19570976099943493, 86.29171490190961435 ) ) ;
#12536 = ORIENTED_EDGE ( 'NONE', *, *, #11106, .F. ) ;
#12537 = EDGE_CURVE ( 'NONE', #2943, #9719, #3565, .T. ) ;
#12538 = UNCERTAINTY_MEASURE_WITH_UNIT (LENGTH_MEASURE( 1.000000000000000082E-05 ), #11679, 'distance_accuracy_value', 'NONE');
#12539 = DIRECTION ( 'NONE',  ( 0.000000000000000000, 0.000000000000000000, -1.000000000000000000 ) ) ;
#12540 = VERTEX_POINT ( 'NONE', #7439 ) ;
#12541 = EDGE_CURVE ( 'NONE', #1127, #5241, #12388, .T. ) ;
#12542 = NEXT_ASSEMBLY_USAGE_OCCURRENCE ( 'NAUO1', ' ', ' ', #5279, #5124, $ ) ;
#12543 = NEXT_ASSEMBLY_USAGE_OCCURRENCE ( 'NAUO2', ' ', ' ', #5279, #7910, $ ) ;
#12544 = NEXT_ASSEMBLY_USAGE_OCCURRENCE ( 'NAUO3', ' ', ' ', #5279, #5438, $ ) ;
#12545 = NEXT_ASSEMBLY_USAGE_OCCURRENCE ( 'NAUO4', ' ', ' ', #5279, #240, $ ) ;
#12546 = NEXT_ASSEMBLY_USAGE_OCCURRENCE ( 'NAUO5', ' ', ' ', #5279, #10161, $ ) ;
#12547 = NEXT_ASSEMBLY_USAGE_OCCURRENCE ( 'NAUO6', ' ', ' ', #5279, #1691, $ ) ;
#12548 = NEXT_ASSEMBLY_USAGE_OCCURRENCE ( 'NAUO7', ' ', ' ', #5279, #1691, $ ) ;
#12549 = NEXT_ASSEMBLY_USAGE_OCCURRENCE ( 'NAUO8', ' ', ' ', #5279, #771, $ ) ;
#12550 = NEXT_ASSEMBLY_USAGE_OCCURRENCE ( 'NAUO9', ' ', ' ', #5279, #10161, $ ) ;
#12551 = NEXT_ASSEMBLY_USAGE_OCCURRENCE ( 'NAUO10', ' ', ' ', #5279, #9616, $ ) ;
#12552 = NEXT_ASSEMBLY_USAGE_OCCURRENCE ( 'NAUO11', ' ', ' ', #5279, #10161, $ ) ;
#12553 = NEXT_ASSEMBLY_USAGE_OCCURRENCE ( 'NAUO12', ' ', ' ', #5279, #10161, $ ) ;
#12554 = NEXT_ASSEMBLY_USAGE_OCCURRENCE ( 'NAUO13', ' ', ' ', #5279, #9616, $ ) ;
#12555 = NEXT_ASSEMBLY_USAGE_OCCURRENCE ( 'NAUO14', ' ', ' ', #5279, #10161, $ ) ;
#12556 = NEXT_ASSEMBLY_USAGE_OCCURRENCE ( 'NAUO15', ' ', ' ', #5279, #10531, $ ) ;
#12557=COLOUR_RGB('Dark Blue',0.08,0.2,0.34);
#12558=FILL_AREA_STYLE_COLOUR('',#12557);
#12559=FILL_AREA_STYLE('',(#12558));
#12560=SURFACE_STYLE_FILL_AREA(#12559);
#12561=SURFACE_SIDE_STYLE('',(#12560));
#12562=SURFACE_STYLE_USAGE(.BOTH.,#12561);
#12563=PRESENTATION_STYLE_ASSIGNMENT((#12562));
#12564=COLOUR_RGB('Light Blue',0.38,0.62,0.78);
#12565=FILL_AREA_STYLE_COLOUR('',#12564);
#12566=FILL_AREA_STYLE('',(#12565));
#12567=SURFACE_STYLE_FILL_AREA(#12566);
#12568=SURFACE_SIDE_STYLE('',(#12567));
#12569=SURFACE_STYLE_USAGE(.BOTH.,#12568);
#12570=PRESENTATION_STYLE_ASSIGNMENT((#12569));
#12571=COLOUR_RGB('Sky Blue',0.24,0.69,0.87);
#12572=FILL_AREA_STYLE_COLOUR('',#12571);
#12573=FILL_AREA_STYLE('',(#12572));
#12574=SURFACE_STYLE_FILL_AREA(#12573);
#12575=SURFACE_SIDE_STYLE('',(#12574));
#12576=SURFACE_STYLE_USAGE(.BOTH.,#12575);
#12577=PRESENTATION_STYLE_ASSIGNMENT((#12576));
#12578=COLOUR_RGB('Grey',0.48,0.52,0.57);
#12579=FILL_AREA_STYLE_COLOUR('',#12578);
#12580=FILL_AREA_STYLE('',(#12579));
#12581=SURFACE_STYLE_FILL_AREA(#12580);
#12582=SURFACE_SIDE_STYLE('',(#12581));
#12583=SURFACE_STYLE_USAGE(.BOTH.,#12582);
#12584=PRESENTATION_STYLE_ASSIGNMENT((#12583));
#12585=COLOUR_RGB('Black',0.12,0.14,0.17);
#12586=FILL_AREA_STYLE_COLOUR('',#12585);
#12587=FILL_AREA_STYLE('',(#12586));
#12588=SURFACE_STYLE_FILL_AREA(#12587);
#12589=SURFACE_SIDE_STYLE('',(#12588));
#12590=SURFACE_STYLE_USAGE(.BOTH.,#12589);
#12591=PRESENTATION_STYLE_ASSIGNMENT((#12590));
#12592=COLOUR_RGB('Off White',0.89,0.88,0.83);
#12593=FILL_AREA_STYLE_COLOUR('',#12592);
#12594=FILL_AREA_STYLE('',(#12593));
#12595=SURFACE_STYLE_FILL_AREA(#12594);
#12596=SURFACE_SIDE_STYLE('',(#12595));
#12597=SURFACE_STYLE_USAGE(.BOTH.,#12596);
#12598=PRESENTATION_STYLE_ASSIGNMENT((#12597));
ENDSEC;
END-ISO-10303-21;
